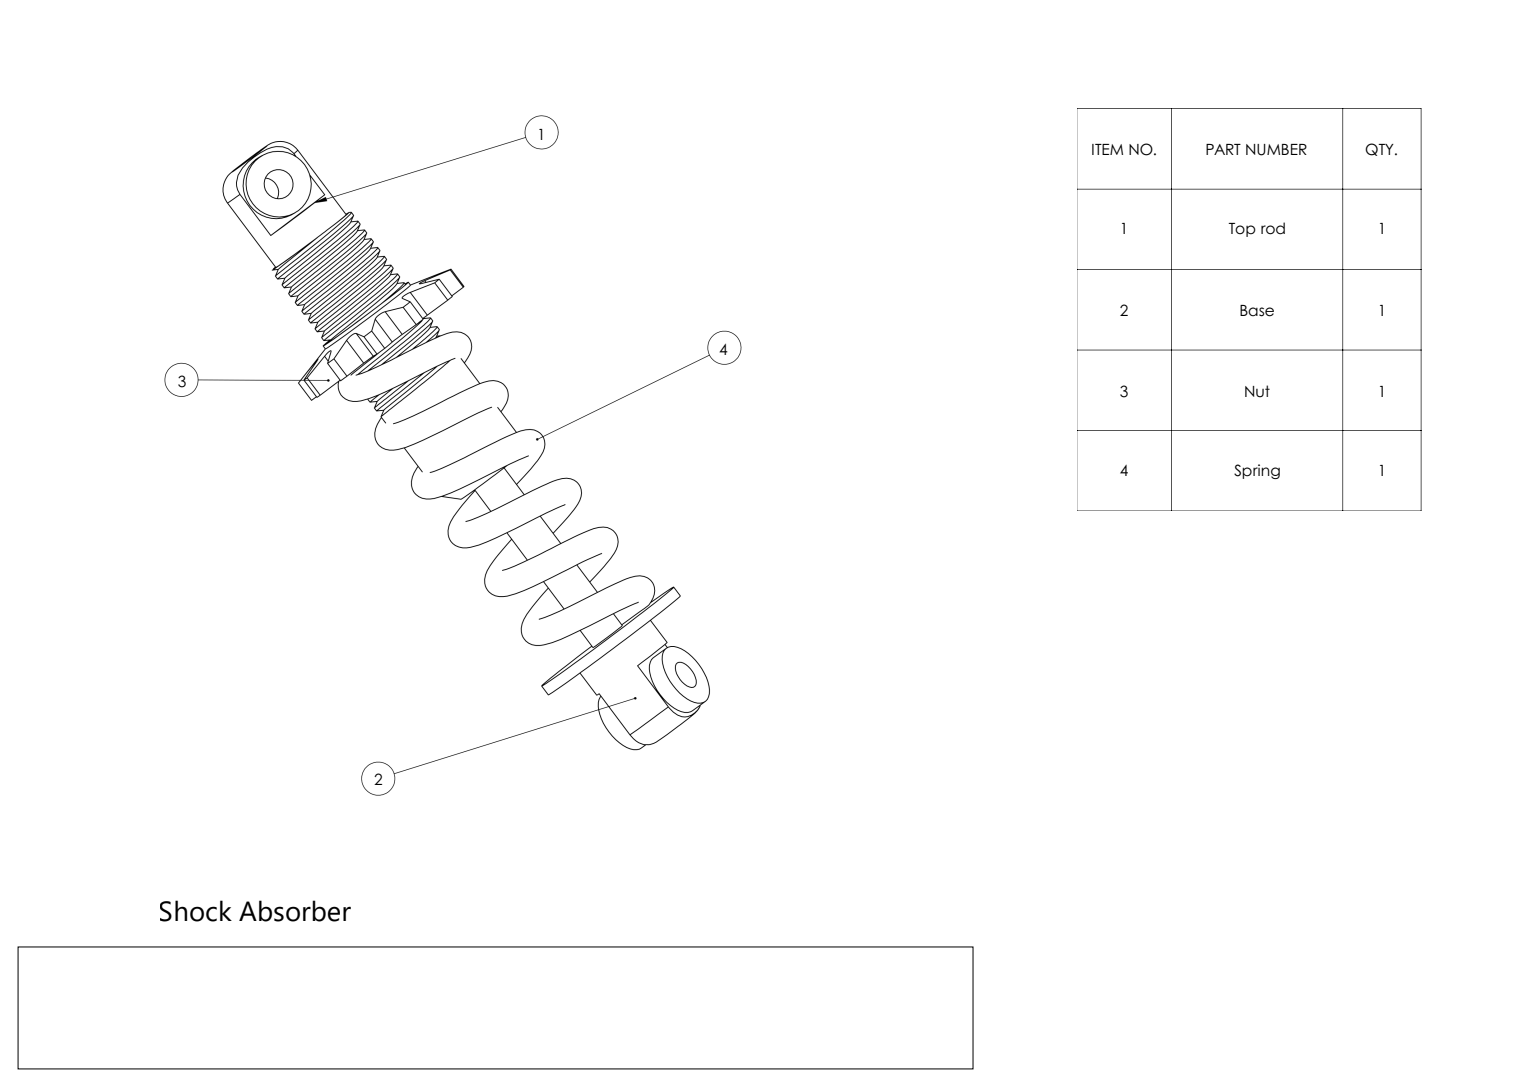
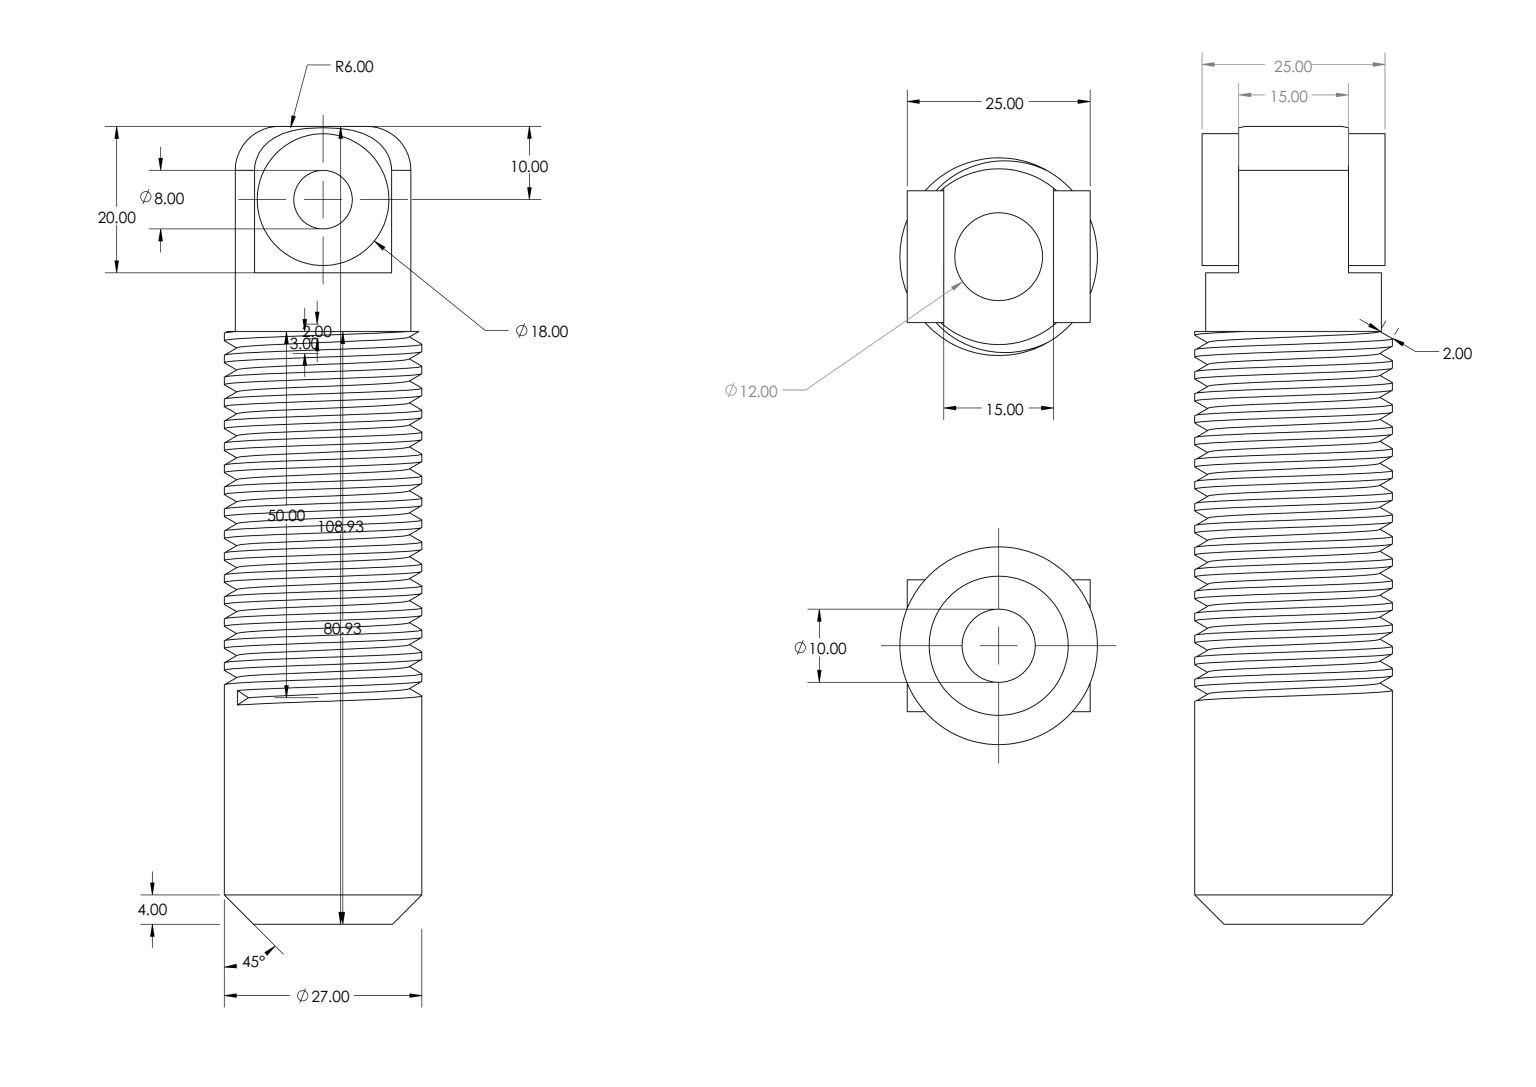
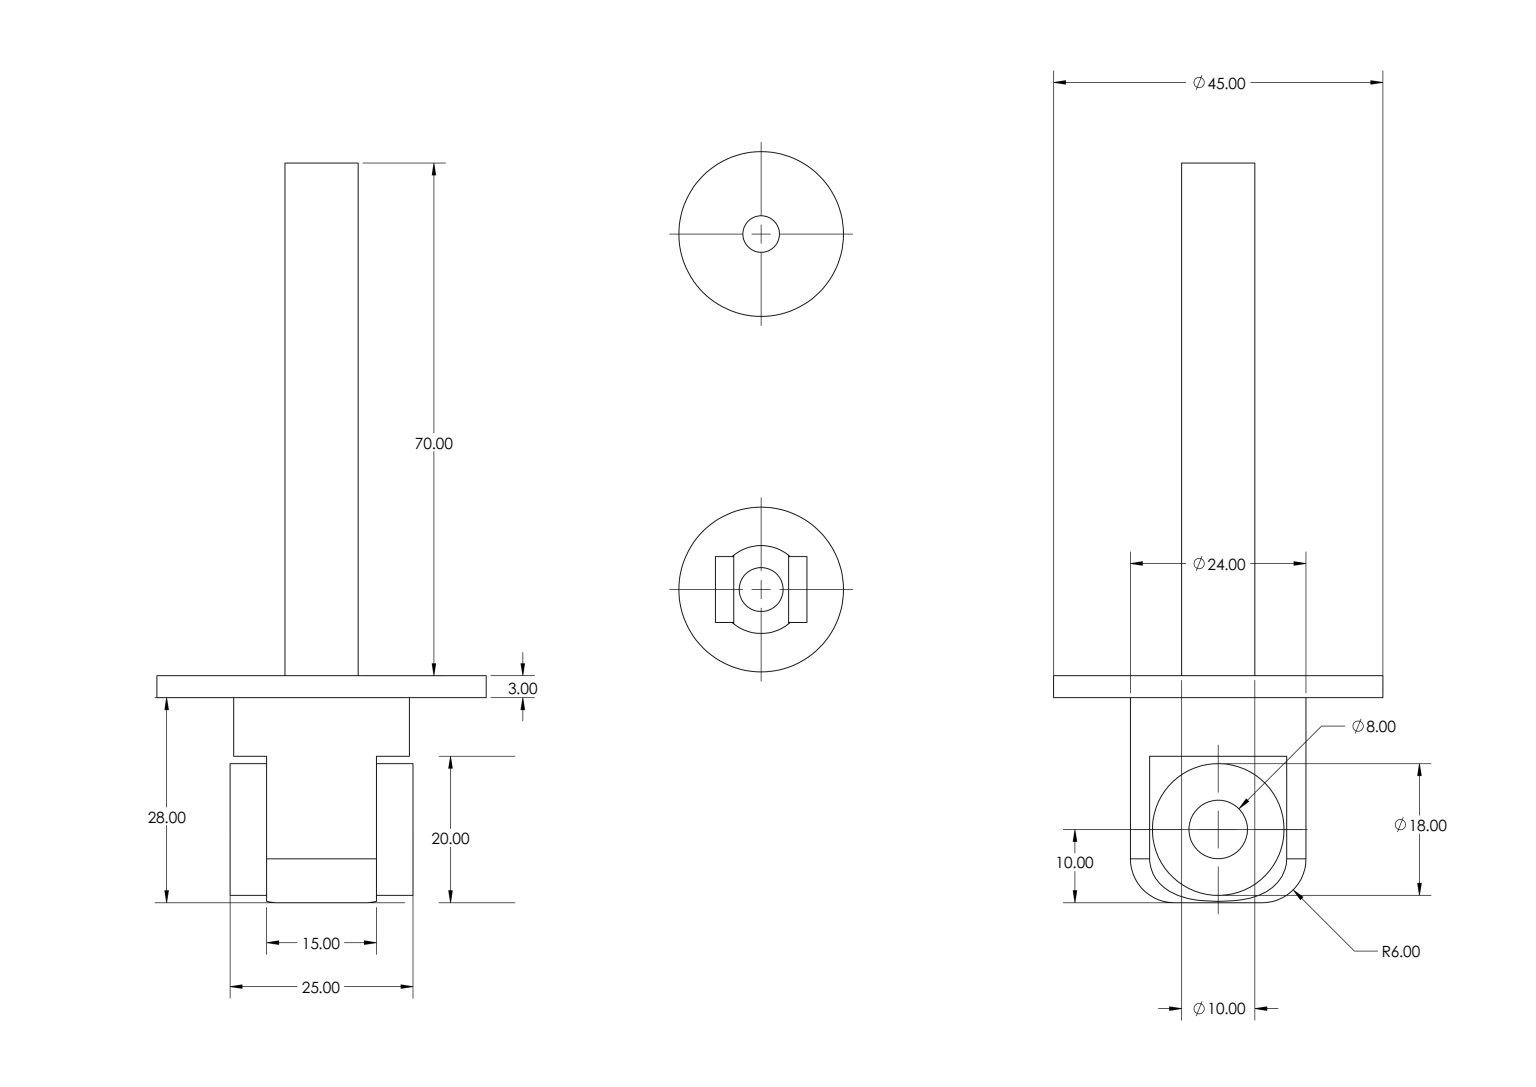
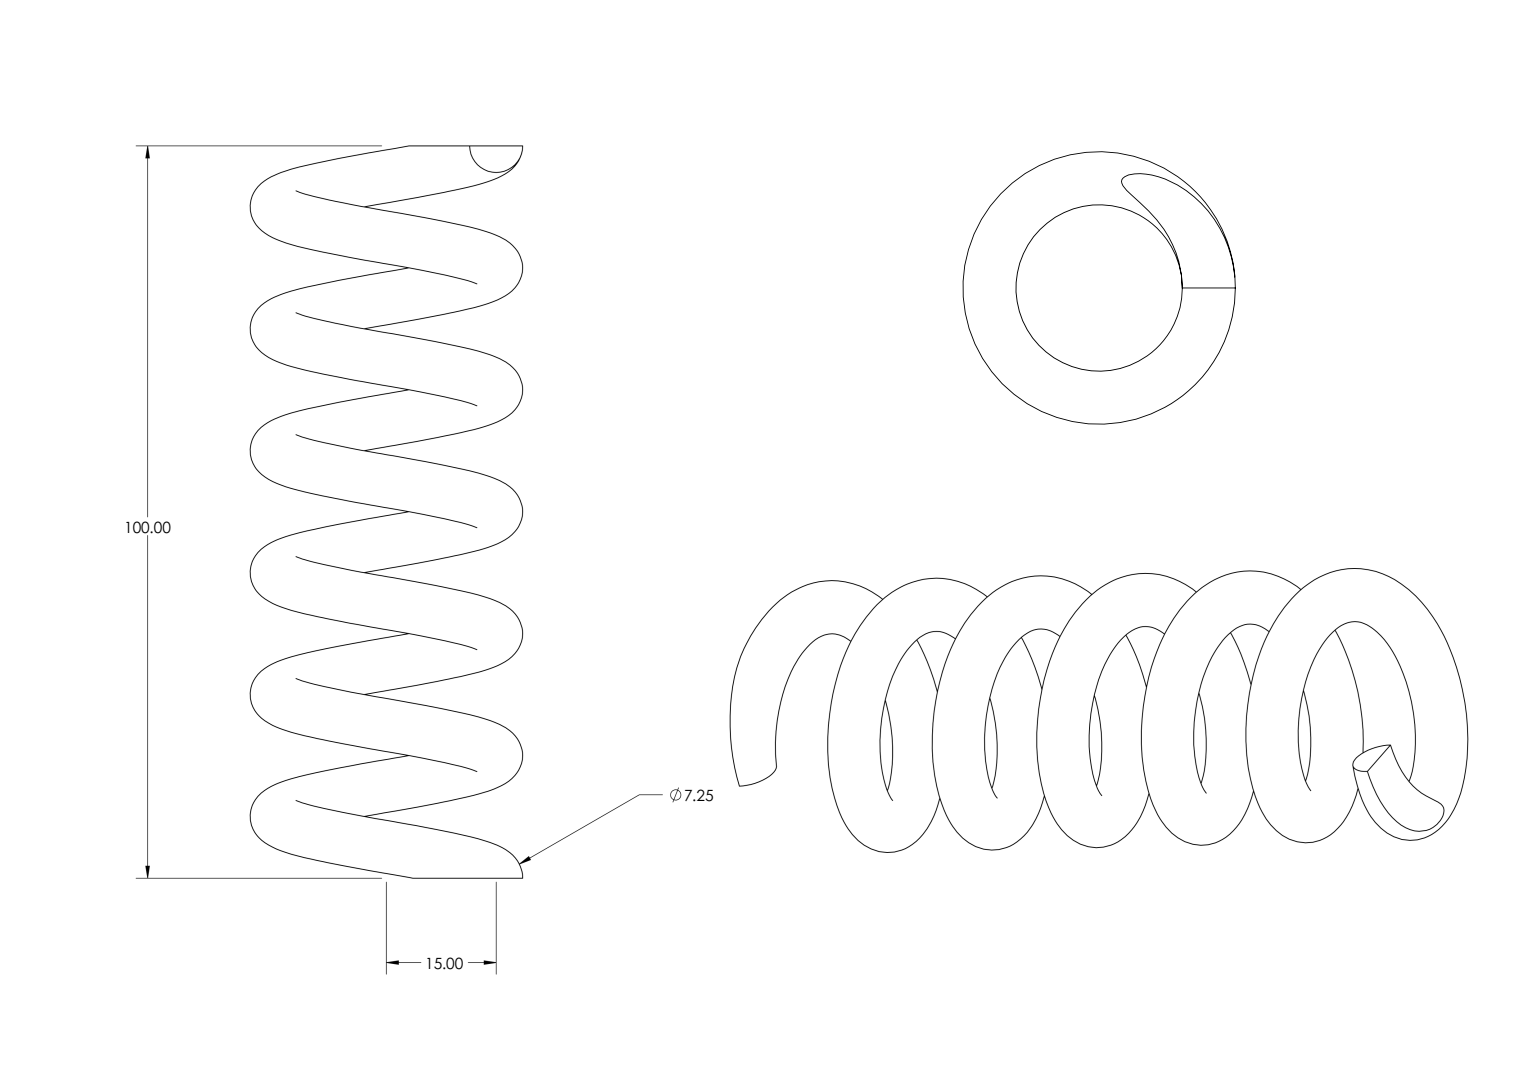
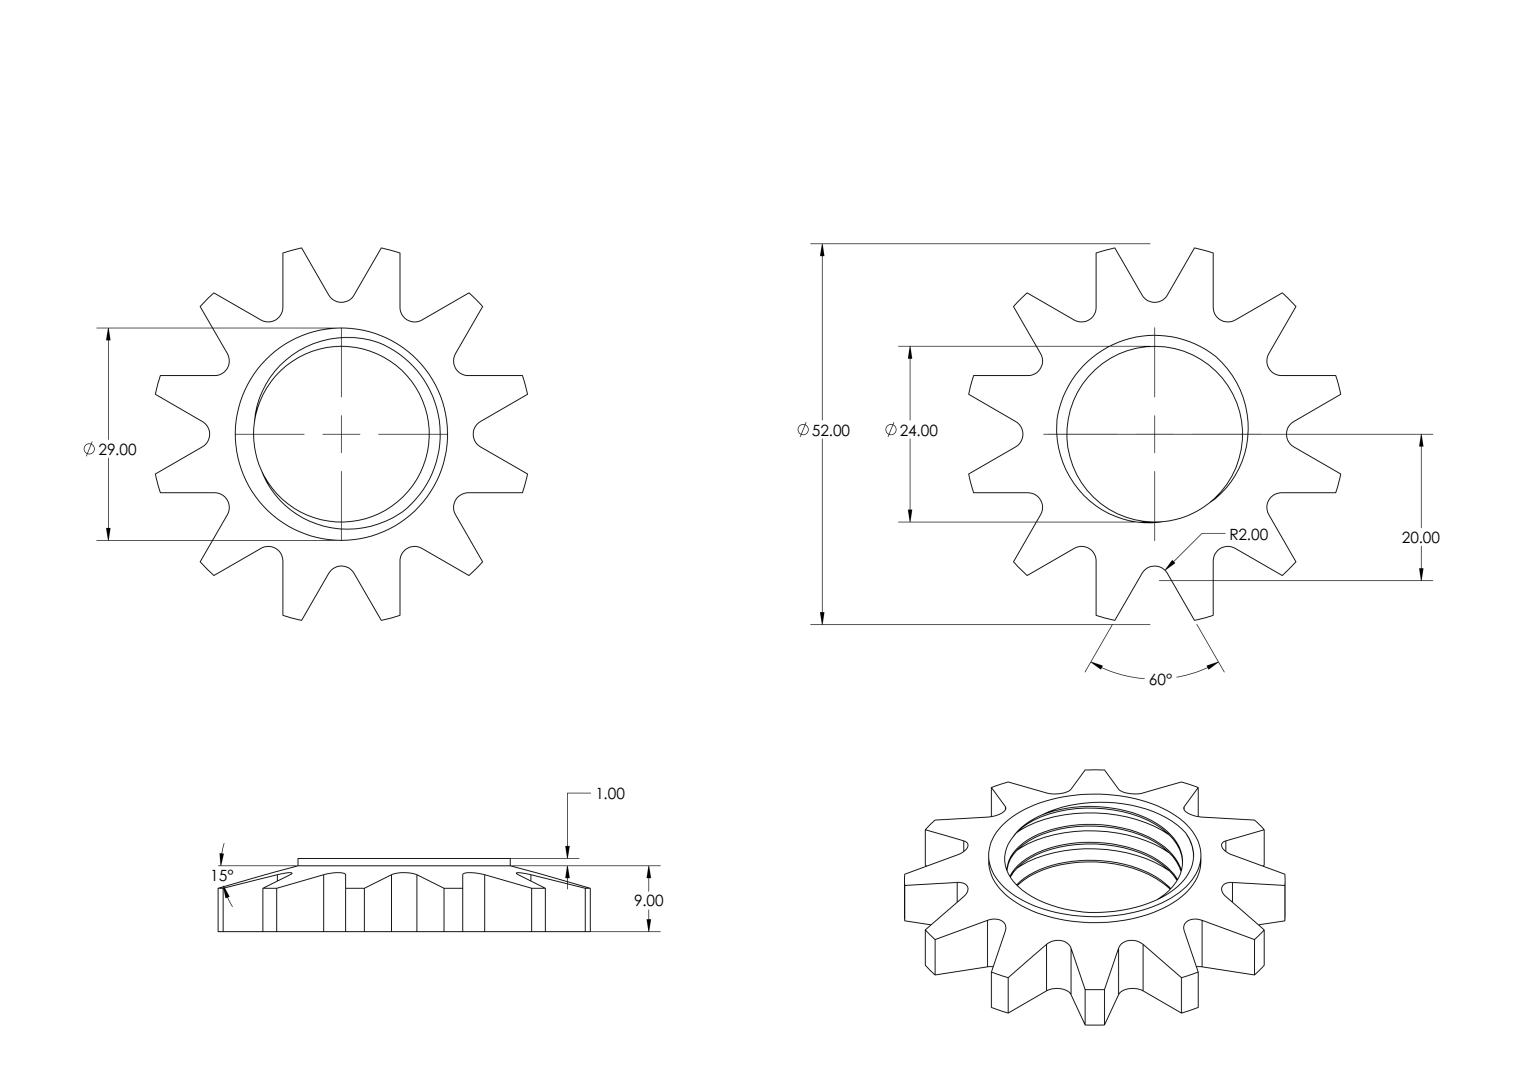
ISO-10303-21;
HEADER;
FILE_DESCRIPTION (('STEP AP214'),
    '1' );
FILE_NAME ('MAT-049',
    '2026-10-21T18:31:44',
    ( '' ),
    ( '' ),
    'SwSTEP 2.0',
    'SolidWorks 2025',
    '' );
FILE_SCHEMA (( 'AUTOMOTIVE_DESIGN' ));
ENDSEC;

DATA;
#1 = CARTESIAN_POINT ( 'NONE',  ( 6.241811971030540640, 75.95141910118948658, -11.97037661190906910 ) ) ;
#2 = CARTESIAN_POINT ( 'NONE',  ( 12.50000000000000000, 98.93000000000002103, 1.224646799147353059E-15 ) ) ;
#3 = CARTESIAN_POINT ( 'NONE',  ( 7.272992578804308828, 36.97999999999998977, 10.01041549318726709 ) ) ;
#4 = CARTESIAN_POINT ( 'NONE',  ( -4.562425571675021274, 41.51584201689734499, 12.70716777987128054 ) ) ;
#5 = CARTESIAN_POINT ( 'NONE',  ( -12.91556685892874867, 58.78902204722160718, -3.932462553950937689 ) ) ;
#6 = CARTESIAN_POINT ( 'NONE',  ( 4.630764260054621495, 44.84669919125740734, 12.68093428297014569 ) ) ;
#7 = CARTESIAN_POINT ( 'NONE',  ( -10.92172942406178926, 54.62999999999999545, -7.935100905948389460 ) ) ;
#8 = CARTESIAN_POINT ( 'NONE',  ( 8.860164440870203606, 30.02243855473401979, 10.18733757369393267 ) ) ;
#9 = ADVANCED_FACE ( 'NONE', ( #480 ), #9607, .F. ) ;
#10 = CARTESIAN_POINT ( 'NONE',  ( -27.07453251570901642, -8.000000000000003553, -22.50000000000000355 ) ) ;
#11 = CARTESIAN_POINT ( 'NONE',  ( -7.522916883230899465, 49.46192173470914355, -11.20972055436655523 ) ) ;
#12 = CARTESIAN_POINT ( 'NONE',  ( 10.11047073980464361, 63.77503176193906143, -8.949362642739272289 ) ) ;
#13 = CARTESIAN_POINT ( 'NONE',  ( 10.29443543732497979, 42.76512297172600796, -8.733575356815638457 ) ) ;
#14 = CARTESIAN_POINT ( 'NONE',  ( 1.387885517463281371, 38.72990328888538869, 13.42850322618521552 ) ) ;
#15 = EDGE_LOOP ( 'NONE', ( #14246, #2278, #8260, #10211 ) ) ;
#16 = DIRECTION ( 'NONE',  ( 0.000000000000000000, 0.000000000000000000, -1.000000000000000000 ) ) ;
#17 = CARTESIAN_POINT ( 'NONE',  ( -10.92172942406179104, 49.23000000000000398, 7.935100905948387684 ) ) ;
#18 = EDGE_LOOP ( 'NONE', ( #8634, #13740, #2829, #14978 ) ) ;
#19 = VERTEX_POINT ( 'NONE', #8191 ) ;
#20 = CARTESIAN_POINT ( 'NONE',  ( -8.549982208541774191E-16, 26.68000000000000682, 14.19474002721660355 ) ) ;
#21 = CARTESIAN_POINT ( 'NONE',  ( -13.16986379959834252, -72.84374999999981526, -13.16986379960055054 ) ) ;
#22 = CARTESIAN_POINT ( 'NONE',  ( 4.958471358563230069, 61.00121407256968098, -12.55670518402642521 ) ) ;
#23 = CARTESIAN_POINT ( 'NONE',  ( -4.171729424061787483, 8.330000000000003624, -12.83926296998457417 ) ) ;
#24 = CARTESIAN_POINT ( 'NONE',  ( 10.50943839410675196, 72.10666813338646364, 8.474155960609857985 ) ) ;
#25 = CARTESIAN_POINT ( 'NONE',  ( 12.25135822064244628, 57.63786423219936239, -5.672709418904434031 ) ) ;
#26 = CARTESIAN_POINT ( 'NONE',  ( 11.76794919243112325, 70.43000000000000682, 1.441158131103945434E-15 ) ) ;
#27 = CARTESIAN_POINT ( 'NONE',  ( 9.520470885617715595, 76.13000000000000966, 6.917026985038134512 ) ) ;
#28 = CARTESIAN_POINT ( 'NONE',  ( -7.237012465003837214, 47.41034925122353627, 11.39682853042513422 ) ) ;
#29 = CARTESIAN_POINT ( 'NONE',  ( -10.92172942406178926, 45.62999999999999545, -7.935100905948389460 ) ) ;
#30 = CARTESIAN_POINT ( 'NONE',  ( 7.347880794884122694E-16, 0.000000000000000000, -20.00000000000000000 ) ) ;
#31 = CARTESIAN_POINT ( 'NONE',  ( 10.92172942406178926, 38.12999999999999545, 7.935100905948387684 ) ) ;
#32 = CARTESIAN_POINT ( 'NONE',  ( 15.00000000000000000, -99.89999999999999147, 0.000000000000000000 ) ) ;
#33 = CARTESIAN_POINT ( 'NONE',  ( -11.37500000000000178, -84.32499999999977547, -9.545674412382054647E-13 ) ) ;
#34 =( BOUNDED_CURVE ( )  B_SPLINE_CURVE ( 2, ( #9058, #4723, #3556 ),
 .UNSPECIFIED., .F., .F. ) 
 B_SPLINE_CURVE_WITH_KNOTS ( ( 3, 3 ),
 ( 0.6250000000000000000, 0.6258333417219855699 ),
 .UNSPECIFIED. ) 
 CURVE ( )  GEOMETRIC_REPRESENTATION_ITEM ( )  RATIONAL_B_SPLINE_CURVE ( ( 0.9755282581475768211, 0.9755282581475767101, 0.9777307592560633420 ) ) 
 REPRESENTATION_ITEM ( '' )  );
#35 = CARTESIAN_POINT ( 'NONE',  ( 13.49999999999999822, 6.279999999999996696, 4.386415899144236796 ) ) ;
#36 = CARTESIAN_POINT ( 'NONE',  ( 11.39480283653290194, 33.70102987876868639, -7.239802240102667596 ) ) ;
#37 = CARTESIAN_POINT ( 'NONE',  ( -4.107118796296879815, 73.32755911965604412, -12.86190453662493383 ) ) ;
#38 = ORIENTED_EDGE ( 'NONE', *, *, #7659, .T. ) ;
#39 = VERTEX_POINT ( 'NONE', #5535 ) ;
#40 = CARTESIAN_POINT ( 'NONE',  ( 11.76794919243112680, 26.57999999999999829, -3.823638476888993942 ) ) ;
#41 = CARTESIAN_POINT ( 'NONE',  ( -2.167727191357447403, 62.60205656133668839, 13.32483508987561649 ) ) ;
#42 = VERTEX_POINT ( 'NONE', #221 ) ;
#43 = CARTESIAN_POINT ( 'NONE',  ( -13.33648623469416528, 41.00345850548239213, 2.095001394486209367 ) ) ;
#44 = CARTESIAN_POINT ( 'NONE',  ( 9.520470885617717371, -12.26999999999999602, -6.917026985038131848 ) ) ;
#45 = CARTESIAN_POINT ( 'NONE',  ( 8.043339635996298753, -88.41874999999980389, 8.043339635997652337 ) ) ;
#46 = CARTESIAN_POINT ( 'NONE',  ( -12.68486621467936359, 44.09791772264757270, 4.641127458682580809 ) ) ;
#47 = CARTESIAN_POINT ( 'NONE',  ( 12.50000000000000000, 98.93000000000002103, 1.224646799147353059E-15 ) ) ;
#48 = PRODUCT_DEFINITION ( 'UNKNOWN', '', #15519, #4010 ) ;
#49 = CARTESIAN_POINT ( 'NONE',  ( -4.171729424061787483, 46.32999999999999829, -12.83926296998457417 ) ) ;
#50 = CARTESIAN_POINT ( 'NONE',  ( 10.92172942406178926, 44.13000000000000256, 7.935100905948387684 ) ) ;
#51 = CARTESIAN_POINT ( 'NONE',  ( -12.09611347903164891, 71.15127006308296131, 6.013594338244640625 ) ) ;
#52 = CARTESIAN_POINT ( 'NONE',  ( 7.714727599200456254, -45.82187499999987779, -18.62499999999935341 ) ) ;
#53 = EDGE_CURVE ( 'NONE', #3761, #17169, #15927, .T. ) ;
#54 = CARTESIAN_POINT ( 'NONE',  ( -13.10508471444031287, 68.04691603053561266, 3.289941233735407256 ) ) ;
#55 = CARTESIAN_POINT ( 'NONE',  ( -7.714727599197334307, 2.046875000000014211, -18.62500000000064659 ) ) ;
#56 = EDGE_CURVE ( 'NONE', #7801, #2957, #9184, .T. ) ;
#57 = CARTESIAN_POINT ( 'NONE',  ( 13.49788837497377969, 54.40198127425698971, 0.8139535183936712492 ) ) ;
#58 = DIRECTION ( 'NONE',  ( -0.000000000000000000, -1.000000000000000000, -0.000000000000000000 ) ) ;
#59 = CARTESIAN_POINT ( 'NONE',  ( -11.88785451664102411, 64.69331280751505631, -6.397572128427487570 ) ) ;
#60 = DIRECTION ( 'NONE',  ( 0.4999999999999977240, 0.000000000000000000, 0.8660254037844399289 ) ) ;
#61 = CARTESIAN_POINT ( 'NONE',  ( -13.32240026865723692, 35.00664116012176663, 2.183159191248645659 ) ) ;
#62 = CARTESIAN_POINT ( 'NONE',  ( 10.92172942406179104, 19.72999999999999687, -7.935100905948385908 ) ) ;
#63 = ORIENTED_EDGE ( 'NONE', *, *, #6522, .T. ) ;
#64 = CARTESIAN_POINT ( 'NONE',  ( -12.94117117538681683, 4.250271015223984582E-15, -2.797136868549697564 ) ) ;
#65 = CARTESIAN_POINT ( 'NONE',  ( -1.332730275901221395, 31.22788502858077209, -13.43591754810035432 ) ) ;
#66 = CARTESIAN_POINT ( 'NONE',  ( 2.964303633682398686, 73.07342191280697818, -13.17196784541496513 ) ) ;
#67 = CARTESIAN_POINT ( 'NONE',  ( -11.76794919243112325, -7.919999999999998153, 3.823638476888994386 ) ) ;
#68 = DIRECTION ( 'NONE',  ( 0.000000000000000000, 0.000000000000000000, 1.000000000000000000 ) ) ;
#69 = CARTESIAN_POINT ( 'NONE',  ( -4.171729424061791036, -11.47000000000000064, 12.83926296998457239 ) ) ;
#70 = CARTESIAN_POINT ( 'NONE',  ( -12.68834643456797906, 52.76331015659336998, -4.610928276790117408 ) ) ;
#71 = CIRCLE ( 'NONE', #15856, 9.000000000000000000 ) ;
#72 = CARTESIAN_POINT ( 'NONE',  ( 9.520470885617715595, 46.12999999999999545, 6.917026985038134512 ) ) ;
#73 = CARTESIAN_POINT ( 'NONE',  ( 3.294673121883986422, 50.79846311650262436, 13.09179671531762246 ) ) ;
#74 = CARTESIAN_POINT ( 'NONE',  ( -9.961542587724716569, 37.57728390915936956, -9.113131270120877758 ) ) ;
#75 = EDGE_CURVE ( 'NONE', #10985, #13128, #6860, .T. ) ;
#76 = CARTESIAN_POINT ( 'NONE',  ( 10.08038093372313604, 36.08304225860660353, 8.991274832604577938 ) ) ;
#77 = CARTESIAN_POINT ( 'NONE',  ( 8.043339635996298753, -105.0687499999997527, 8.043339635997652337 ) ) ;
#78 = CARTESIAN_POINT ( 'NONE',  ( -11.44756249950965632, 74.19779003843927967, 7.160551751645796159 ) ) ;
#79 = CARTESIAN_POINT ( 'NONE',  ( -13.19858737197696286, 77.03056283200281484, 2.845309594670863973 ) ) ;
#80 = AXIS2_PLACEMENT_3D ( 'NONE', #263, #10869, #2892 ) ;
#81 = CARTESIAN_POINT ( 'NONE',  ( -6.071462803580223166, 79.40141861843632398, -12.06817019399647783 ) ) ;
#82 = CARTESIAN_POINT ( 'NONE',  ( 2.279995255611139653E-15, 9.179999999999992610, -12.37355403259654985 ) ) ;
#83 = CARTESIAN_POINT ( 'NONE',  ( 13.50000000000000000, 4.430000000000003268, 1.734723475976807094E-15 ) ) ;
#84 = CARTESIAN_POINT ( 'NONE',  ( 1.982521523170245906E-06, 77.68005525700222336, 13.49999999999970690 ) ) ;
#85 = CARTESIAN_POINT ( 'NONE',  ( 11.76794919243112680, -0.4200000000000027045, -3.823638476888993942 ) ) ;
#86 = CARTESIAN_POINT ( 'NONE',  ( 3.636496289402154414, 51.82999999999999829, 11.19198476289190936 ) ) ;
#87 = CARTESIAN_POINT ( 'NONE',  ( 8.043339635997654113, -18.73124999999995666, -8.043339635996304082 ) ) ;
#88 = CARTESIAN_POINT ( 'NONE',  ( -13.16986379960055231, -43.70624999999989768, 13.16986379959834252 ) ) ;
#89 = CARTESIAN_POINT ( 'NONE',  ( -10.92172942406179104, -12.76999999999999602, 7.935100905948385908 ) ) ;
#90 = CARTESIAN_POINT ( 'NONE',  ( -8.290587820170616240, 40.49598020429036183, -10.65487298274420525 ) ) ;
#91 = CARTESIAN_POINT ( 'NONE',  ( -2.747897566831316141, 34.27880424421546479, -13.21738048412783151 ) ) ;
#92 = CARTESIAN_POINT ( 'NONE',  ( 13.48604648626630542, 75.45114278836371113, -0.6137407349411325708 ) ) ;
#93 = CARTESIAN_POINT ( 'NONE',  ( 15.91271015948297141, 2.066541229842319115E-14, -9.178967570126440378 ) ) ;
#94 = CARTESIAN_POINT ( 'NONE',  ( -11.76794919243112325, 32.92999999999999972, -2.882316262207890869E-15 ) ) ;
#95 = CARTESIAN_POINT ( 'NONE',  ( -6.586690174280394494, 41.43750565762731952, 11.78692872275349579 ) ) ;
#96 = CARTESIAN_POINT ( 'NONE',  ( -4.171426067996565124, 58.32999100947719029, -12.83948131572000584 ) ) ;
#97 = CARTESIAN_POINT ( 'NONE',  ( 6.370293526262202022, 44.91380087981439573, 11.90272333445460262 ) ) ;
#98 = ADVANCED_FACE ( 'NONE', ( #16379 ), #12591, .T. ) ;
#99 = CARTESIAN_POINT ( 'NONE',  ( -17.32050807568884210, 7.773118517290098950, 7.999999999999840128 ) ) ;
#100 = CARTESIAN_POINT ( 'NONE',  ( 1.108954987895778950E-11, 4.813974596216015200, 12.00000000000000178 ) ) ;
#101 = CARTESIAN_POINT ( 'NONE',  ( -4.171729424061791036, 58.53000000000000114, 12.83926296998457239 ) ) ;
#102 = CARTESIAN_POINT ( 'NONE',  ( -11.20551244324089524, 49.64703832191597854, -7.529055542132852885 ) ) ;
#103 = CARTESIAN_POINT ( 'NONE',  ( 13.46801799936566724, 63.39787863554747815, 0.9304553811726751222 ) ) ;
#104 = CARTESIAN_POINT ( 'NONE',  ( 11.68815242529539411, 42.17840658691920908, 6.773979411268512330 ) ) ;
#105 = CARTESIAN_POINT ( 'NONE',  ( 4.417203864861311224, 38.83887425577129449, 12.75710294833973357 ) ) ;
#106 = VERTEX_POINT ( 'NONE', #2759 ) ;
#107 = CARTESIAN_POINT ( 'NONE',  ( -4.026122579657434919, 70.32476532614168718, -12.88571505164192033 ) ) ;
#108 = CARTESIAN_POINT ( 'NONE',  ( -13.49999999999999822, 48.77999999999998693, -4.386415899144240349 ) ) ;
#109 = CARTESIAN_POINT ( 'NONE',  ( -8.343458848123582072, 14.37999999999998835, 11.48378591275254124 ) ) ;
#110 = EDGE_LOOP ( 'NONE', ( #6207, #1537, #1550, #818 ) ) ;
#111 = CARTESIAN_POINT ( 'NONE',  ( -4.477815178396856055, 43.34114203380904229, -12.73627368523690606 ) ) ;
#112 = DIRECTION ( 'NONE',  ( -0.000000000000000000, -1.000000000000000000, -0.000000000000000000 ) ) ;
#113 = CARTESIAN_POINT ( 'NONE',  ( 6.392086272904786703, 60.94536626219394293, -11.89080869004308205 ) ) ;
#114 = CARTESIAN_POINT ( 'NONE',  ( -8.343458848123576743, 14.47999999999999865, -11.48378591275254301 ) ) ;
#115 = CARTESIAN_POINT ( 'NONE',  ( 2.453092984686562339, 71.76820780413271450, 13.27525308931726578 ) ) ;
#116 = CARTESIAN_POINT ( 'NONE',  ( 13.40373713238982489, 66.48610201136790465, -1.609300758946977661 ) ) ;
#117 = CARTESIAN_POINT ( 'NONE',  ( 4.966293671374200969, 56.85915651247563574, 12.55332637815666708 ) ) ;
#118 = CARTESIAN_POINT ( 'NONE',  ( 3.636496289402154414, 66.82999999999999829, 11.19198476289190936 ) ) ;
#119 = CARTESIAN_POINT ( 'NONE',  ( 9.520470885617715595, 64.12999999999999545, 6.917026985038134512 ) ) ;
#120 = CARTESIAN_POINT ( 'NONE',  ( -3.966664967154714727, 47.53736456333449922, 12.90422583550607527 ) ) ;
#121 = CARTESIAN_POINT ( 'NONE',  ( -13.49999999999999822, 45.78000000000000114, -4.386415899144240349 ) ) ;
#122 = CARTESIAN_POINT ( 'NONE',  ( -8.224360503536546367E-15, 78.17999999999999261, -13.50000000000000000 ) ) ;
#123 = CARTESIAN_POINT ( 'NONE',  ( 4.163872747629839388, -100.0000000000000426, 15.14667126703698585 ) ) ;
#124 = CARTESIAN_POINT ( 'NONE',  ( -3.802315511192875697, 56.54328190446157976, 12.95363457325665202 ) ) ;
#125 = CARTESIAN_POINT ( 'NONE',  ( -11.37500000000000000, -41.62499999999990052, -9.545674412382054647E-13 ) ) ;
#126 = CARTESIAN_POINT ( 'NONE',  ( -4.171729424061791036, 40.52999999999999403, 12.83926296998457239 ) ) ;
#127 = AXIS2_PLACEMENT_3D ( 'NONE', #2848, #1623, #9520 ) ;
#128 = CARTESIAN_POINT ( 'NONE',  ( 13.48850798719686317, 33.44917238739969889, -0.5569197484580091784 ) ) ;
#129 = CARTESIAN_POINT ( 'NONE',  ( -13.14483242576192978, 7.170662809914418290, -16.82677684650047567 ) ) ;
#130 = EDGE_LOOP ( 'NONE', ( #12331, #307, #5558 ) ) ;
#131 = EDGE_LOOP ( 'NONE', ( #5447, #10898, #7879, #3829 ) ) ;
#132 = CARTESIAN_POINT ( 'NONE',  ( -2.372100534622330059, 62.59470822479858043, 13.29057958102706571 ) ) ;
#133 = ORIENTED_EDGE ( 'NONE', *, *, #911, .F. ) ;
#134 = B_SPLINE_CURVE_WITH_KNOTS ( 'NONE', 3,
 ( #15432, #7424, #3341, #16438 ),
 .UNSPECIFIED., .F., .F.,
 ( 4, 4 ),
 ( 2.376698214938428888E-07, 0.007646667280170321192 ),
 .UNSPECIFIED. ) ;
#135 = CARTESIAN_POINT ( 'NONE',  ( -11.76794919243112325, -14.22000000000000242, -3.823638476888998827 ) ) ;
#136 = CARTESIAN_POINT ( 'NONE',  ( 13.16986379960055409, -42.63124999999990905, -13.16986379959834430 ) ) ;
#137 = CARTESIAN_POINT ( 'NONE',  ( -13.22798356179965751, 44.02531610866294187, 2.697370474855687927 ) ) ;
#138 = CARTESIAN_POINT ( 'NONE',  ( 7.999999999999904965, 7.773118517290098950, 17.32050807568881368 ) ) ;
#139 = EDGE_CURVE ( 'NONE', #3044, #15045, #14019, .T. ) ;
#140 = CARTESIAN_POINT ( 'NONE',  ( 13.50000000000000355, 42.57999999999999829, -4.386415899144233244 ) ) ;
#141 = CARTESIAN_POINT ( 'NONE',  ( -13.50000000000000000, 48.92999999999999972, -3.306546357697853733E-15 ) ) ;
#142 = CARTESIAN_POINT ( 'NONE',  ( -13.48995242675199790, 70.94917795696534313, 0.5552773507619721549 ) ) ;
#143 =( BOUNDED_CURVE ( )  B_SPLINE_CURVE ( 1, ( #8817, #14343 ),
 .UNSPECIFIED., .F., .F. ) 
 B_SPLINE_CURVE_WITH_KNOTS ( ( 2, 2 ),
 ( 0.000000000000000000, 1.000000000000000000 ),
 .UNSPECIFIED. ) 
 CURVE ( )  GEOMETRIC_REPRESENTATION_ITEM ( )  RATIONAL_B_SPLINE_CURVE ( ( 0.9782075210486875783, 0.9782075210486875783 ) ) 
 REPRESENTATION_ITEM ( '' )  );
#144 = CARTESIAN_POINT ( 'NONE',  ( -13.16986379959834252, -65.59374999999981526, -13.16986379960055409 ) ) ;
#145 = CARTESIAN_POINT ( 'NONE',  ( -11.47846244632648549, 67.66437547590606982, -7.110784611987690518 ) ) ;
#146 = CARTESIAN_POINT ( 'NONE',  ( 18.62500000000000000, -75.99999999999980105, 1.560692158462880521E-12 ) ) ;
#147 = CARTESIAN_POINT ( 'NONE',  ( 12.45812093344438587, 54.62011758101717618, -5.223734028880926417 ) ) ;
#148 = CARTESIAN_POINT ( 'NONE',  ( -11.89319909969382039, 64.69371209007049117, -6.387634285403382073 ) ) ;
#149 = VERTEX_POINT ( 'NONE', #9845 ) ;
#150 = CARTESIAN_POINT ( 'NONE',  ( 15.58845726811991916, 7.773118517290098950, -10.99999999999996092 ) ) ;
#151 = CARTESIAN_POINT ( 'NONE',  ( -12.98939268596651786, 34.79855291303425702, -3.677969189785255555 ) ) ;
#152 = ORIENTED_EDGE ( 'NONE', *, *, #6438, .T. ) ;
#153 = CARTESIAN_POINT ( 'NONE',  ( 13.08478391751391001, 78.54823588313601590, -3.322629509287643224 ) ) ;
#154 = CARTESIAN_POINT ( 'NONE',  ( -13.39378209699495592, -2.969872329747732787E-15, 1.511216576358205943 ) ) ;
#155 = CARTESIAN_POINT ( 'NONE',  ( 0.000000000000000000, 73.00000000000001421, 0.000000000000000000 ) ) ;
#156 = CARTESIAN_POINT ( 'NONE',  ( -9.949531856098463578, 31.57665661914821342, -9.126009350303103673 ) ) ;
#157 = CARTESIAN_POINT ( 'NONE',  ( 10.34601424054412000, 72.76232993950749517, -8.672412499177319489 ) ) ;
#158 = CARTESIAN_POINT ( 'NONE',  ( -7.409984580736203970E-16, -7.320000000000002949, 12.37355403259654985 ) ) ;
#159 = DIRECTION ( 'NONE',  ( 1.000000000000000000, 0.000000000000000000, 0.000000000000000000 ) ) ;
#160 = EDGE_CURVE ( 'NONE', #16949, #8284, #16780, .T. ) ;
#161 = CARTESIAN_POINT ( 'NONE',  ( -4.171729424061791036, -14.46999999999999709, 12.83926296998457239 ) ) ;
#162 = AXIS2_PLACEMENT_3D ( 'NONE', #175, #4418, #13594 ) ;
#163 = CARTESIAN_POINT ( 'NONE',  ( -10.92172942406178926, 70.62999999999999545, -7.935100905948389460 ) ) ;
#164 = CARTESIAN_POINT ( 'NONE',  ( -12.03726189314226858, 53.15526546510770345, 6.112069937274645426 ) ) ;
#165 = CARTESIAN_POINT ( 'NONE',  ( -7.272992578804307939, 44.47999999999999687, -10.01041549318726886 ) ) ;
#166 = CARTESIAN_POINT ( 'NONE',  ( -13.50000000000000000, 69.93000000000000682, -3.306546357697853733E-15 ) ) ;
#167 = CARTESIAN_POINT ( 'NONE',  ( -16.03540712409196090, 8.027799080943070820, -8.457499700851245805 ) ) ;
#168 = CARTESIAN_POINT ( 'NONE',  ( 11.95757905990039127, 69.66142261759961229, -6.266300119430860072 ) ) ;
#169 = CARTESIAN_POINT ( 'NONE',  ( -4.427829777958112167, 37.33925957768354920, -12.75364605705754606 ) ) ;
#170 = CARTESIAN_POINT ( 'NONE',  ( 3.589871069019304972, 35.80905818983445954, 13.01962489795650768 ) ) ;
#171 = CARTESIAN_POINT ( 'NONE',  ( -11.37500000000039613, -83.21562499999981810, 4.711679271993000739 ) ) ;
#172 = CARTESIAN_POINT ( 'NONE',  ( -10.34620055824173868, 74.26233662262045243, 8.672923399463462246 ) ) ;
#173 = CARTESIAN_POINT ( 'NONE',  ( -13.29880297559754609, 76.84835896960053958, -2.322037454927736277 ) ) ;
#174 = DIRECTION ( 'NONE',  ( 0.000000000000000000, -1.000000000000000000, 0.000000000000000000 ) ) ;
#175 = CARTESIAN_POINT ( 'NONE',  ( 0.000000000000000000, 0.000000000000000000, 0.000000000000000000 ) ) ;
#176 = CARTESIAN_POINT ( 'NONE',  ( -8.380961239563070819, 80.93000000000004945, 9.227099233226635278 ) ) ;
#177 = CARTESIAN_POINT ( 'NONE',  ( 13.49999999999999822, 28.28000000000000114, 4.386415899144237684 ) ) ;
#178 = CARTESIAN_POINT ( 'NONE',  ( -11.76794919243112325, 4.080000000000008065, 3.823638476888994386 ) ) ;
#179 = CARTESIAN_POINT ( 'NONE',  ( 9.520470885617715595, 46.12999999999999545, 6.917026985038134512 ) ) ;
#180 = CARTESIAN_POINT ( 'NONE',  ( 13.49999999999999822, -17.72000000000000242, 4.386415899144237684 ) ) ;
#181 = CARTESIAN_POINT ( 'NONE',  ( 6.750022565184456980, 31.92926174983938026, 11.69132992304556495 ) ) ;
#182 = CARTESIAN_POINT ( 'NONE',  ( 10.14927042510883481, 75.08716984626934732, 8.902032665787164234 ) ) ;
#183 = EDGE_CURVE ( 'NONE', #10985, #14307, #6879, .T. ) ;
#184 = CARTESIAN_POINT ( 'NONE',  ( 3.512344863372272030, -7.135244913870580524E-13, -15.22848700163195623 ) ) ;
#185 = VECTOR ( 'NONE', #11440, 1000.000000000000000 ) ;
#186 = CARTESIAN_POINT ( 'NONE',  ( 0.000000000000000000, 0.000000000000000000, 0.000000000000000000 ) ) ;
#187 = CARTESIAN_POINT ( 'NONE',  ( -6.864354898698485918, 41.42600474588421378, 11.62474807620217376 ) ) ;
#188 = CARTESIAN_POINT ( 'NONE',  ( -6.117255243659908359, 58.40366678541308687, -12.03616728541428493 ) ) ;
#189 = FACE_OUTER_BOUND ( 'NONE', #3646, .T. ) ;
#190 = CARTESIAN_POINT ( 'NONE',  ( -4.171729424061787483, 54.33000000000000540, -12.83926296998457417 ) ) ;
#191 = DIRECTION ( 'NONE',  ( -0.000000000000000000, -1.000000000000000000, -0.000000000000000000 ) ) ;
#192 = CARTESIAN_POINT ( 'NONE',  ( -13.49999999999999822, 57.78000000000000114, -4.386415899144240349 ) ) ;
#193 = CARTESIAN_POINT ( 'NONE',  ( -11.00427691244374273, 49.63475489259692353, -7.821558401853768494 ) ) ;
#194 = CARTESIAN_POINT ( 'NONE',  ( 11.36089011803204407, 63.70299262790948802, -7.293906877826991320 ) ) ;
#195 = CARTESIAN_POINT ( 'NONE',  ( 13.46351984225201548, 42.39558882709123111, 0.9962785372066437217 ) ) ;
#196 = CARTESIAN_POINT ( 'NONE',  ( 3.151611543758418676, 38.79326144612200267, 13.13455959399786899 ) ) ;
#197 = ORIENTED_EDGE ( 'NONE', *, *, #1177, .T. ) ;
#198 = CARTESIAN_POINT ( 'NONE',  ( -3.974014160384248928, 70.32289088885870854, -12.90183134154761113 ) ) ;
#199 = CARTESIAN_POINT ( 'NONE',  ( -11.37500000000039613, -9.365624999999976552, 4.711679271993001628 ) ) ;
#200 = CIRCLE ( 'NONE', #2424, 5.000000000000000000 ) ;
#201 = VERTEX_POINT ( 'NONE', #13114 ) ;
#202 = CARTESIAN_POINT ( 'NONE',  ( -11.06052376482290889, 43.63819014080397807, -7.740673448246946364 ) ) ;
#203 = CARTESIAN_POINT ( 'NONE',  ( -7.499999999999999112, 105.5999945338998174, 8.557281619885976909 ) ) ;
#204 = CARTESIAN_POINT ( 'NONE',  ( 10.49915709197846603, 60.75394407136035113, -8.486442428007933358 ) ) ;
#205 = CARTESIAN_POINT ( 'NONE',  ( 13.50000000000000355, 7.579999999999999183, -4.386415899144233244 ) ) ;
#206 = EDGE_CURVE ( 'NONE', #10449, #12592, #1531, .T. ) ;
#207 = CARTESIAN_POINT ( 'NONE',  ( -3.708203932499367195, 6.196025403784440222, -11.41267819554184548 ) ) ;
#208 = CARTESIAN_POINT ( 'NONE',  ( 12.91036043465679128, 66.57159231767617769, -3.948717839537223551 ) ) ;
#209 = CARTESIAN_POINT ( 'NONE',  ( 10.83372828063143523, 57.12494043467410165, 8.055071804621336540 ) ) ;
#210 = CARTESIAN_POINT ( 'NONE',  ( 3.636496289402157078, 62.03000000000000114, -11.19198476289190936 ) ) ;
#211 = CARTESIAN_POINT ( 'NONE',  ( -11.76794919243112325, 71.78000000000000114, -3.823638476888998827 ) ) ;
#212 = CARTESIAN_POINT ( 'NONE',  ( -8.395919747993797699, 47.35978594638820738, 10.59303779737377127 ) ) ;
#213 = CARTESIAN_POINT ( 'NONE',  ( -10.92172942406179104, 46.22999999999999687, 7.935100905948387684 ) ) ;
#214 = FACE_OUTER_BOUND ( 'NONE', #12871, .T. ) ;
#215 = CARTESIAN_POINT ( 'NONE',  ( 3.658660341103826763, -100.0000000000000000, 14.07150118901589408 ) ) ;
#216 = CARTESIAN_POINT ( 'NONE',  ( -9.167797302161076800, 56.32288307047150511, 9.914146655588314871 ) ) ;
#217 = CARTESIAN_POINT ( 'NONE',  ( 8.043339635996300530, -81.16874999999980389, 8.043339635997654113 ) ) ;
#218 = CARTESIAN_POINT ( 'NONE',  ( 2.138189944381238661, 5.756881422320270225, 13.49999999999999822 ) ) ;
#219 = CARTESIAN_POINT ( 'NONE',  ( 12.00723290083941208, 33.65759935958783444, -6.170612997742742856 ) ) ;
#220 = PLANE ( 'NONE',  #1477 ) ;
#221 = CARTESIAN_POINT ( 'NONE',  ( -18.99999999999998224, 0.000000000000000000, -1.732050807569074369 ) ) ;
#222 = CARTESIAN_POINT ( 'NONE',  ( -3.636496289402152637, 24.33000000000001961, -11.19198476289190936 ) ) ;
#223 = ORIENTED_EDGE ( 'NONE', *, *, #9601, .T. ) ;
#224 = CARTESIAN_POINT ( 'NONE',  ( -5.623820243337235958, 62.47578838716487581, 12.27284524967300605 ) ) ;
#225 = VERTEX_POINT ( 'NONE', #3915 ) ;
#226 = CARTESIAN_POINT ( 'NONE',  ( -13.39469296682190347, 40.86889263995428934, -1.754359878167341513 ) ) ;
#227 = CARTESIAN_POINT ( 'NONE',  ( -18.62500000000064659, -16.61562499999998010, 7.714727599197333419 ) ) ;
#228 = CARTESIAN_POINT ( 'NONE',  ( -12.06034990428044118, 44.15344642025849708, 6.066424416400918673 ) ) ;
#229 = CARTESIAN_POINT ( 'NONE',  ( -9.831838144771234411, 8.007813437504038845, 15.31996850146883382 ) ) ;
#230 = CARTESIAN_POINT ( 'NONE',  ( -8.691771469529815392E-16, 38.67999999999999972, 14.19474002721660355 ) ) ;
#231 = CARTESIAN_POINT ( 'NONE',  ( 4.171729424061791924, 45.03000000000000114, -12.83926296998457239 ) ) ;
#232 = CARTESIAN_POINT ( 'NONE',  ( -13.49234022047965809, 70.91385223794031845, -0.4697109487732297195 ) ) ;
#233 = CARTESIAN_POINT ( 'NONE',  ( -7.714727599197334307, -64.55312499999983800, -18.62500000000064659 ) ) ;
#234 = CARTESIAN_POINT ( 'NONE',  ( -11.77082077961090967, 67.68472015259277441, -6.610832368286345684 ) ) ;
#235 = CARTESIAN_POINT ( 'NONE',  ( 18.62499999999935341, -58.30937499999983231, 7.714727599200469577 ) ) ;
#236 = CARTESIAN_POINT ( 'NONE',  ( 10.59104740856127513, 54.74884203901541468, -8.371597748919196391 ) ) ;
#237 = EDGE_CURVE ( 'NONE', #1377, #15607, #758, .T. ) ;
#238 = CARTESIAN_POINT ( 'NONE',  ( -3.290095754100384351, 64.29827642083250794, -13.09294913094749191 ) ) ;
#239 = ORIENTED_EDGE ( 'NONE', *, *, #2811, .F. ) ;
#240 = CARTESIAN_POINT ( 'NONE',  ( -4.171729424061791036, 64.53000000000000114, 12.83926296998457239 ) ) ;
#241 = CARTESIAN_POINT ( 'NONE',  ( -12.55115401018059451, 35.11056623410730992, 4.971969969848257342 ) ) ;
#242 = VECTOR ( 'NONE', #6179, 1000.000000000000000 ) ;
#243 = ORIENTED_EDGE ( 'NONE', *, *, #10979, .T. ) ;
#244 = CARTESIAN_POINT ( 'NONE',  ( 13.49341015684798428, 78.44682598755416336, -0.4906469715254504482 ) ) ;
#245 = CARTESIAN_POINT ( 'NONE',  ( 4.171729424061789260, 49.82999999999999829, 12.83926296998457417 ) ) ;
#246 = CARTESIAN_POINT ( 'NONE',  ( 7.500000000000001776, -24.45288220904212295, 8.693347190813737413 ) ) ;
#247 = CARTESIAN_POINT ( 'NONE',  ( 4.352178298388634126, 73.02340726775082658, -12.78109873716751466 ) ) ;
#248 = FACE_OUTER_BOUND ( 'NONE', #11679, .T. ) ;
#249 = CARTESIAN_POINT ( 'NONE',  ( 8.343458848123578520, -14.02000000000000135, 11.48378591275254124 ) ) ;
#250 = CARTESIAN_POINT ( 'NONE',  ( -8.343458848123582072, 68.38000000000000966, 11.48378591275254124 ) ) ;
#251 = CARTESIAN_POINT ( 'NONE',  ( -11.21331758585850302, 52.64752326776081048, -7.517415214335143148 ) ) ;
#252 = CARTESIAN_POINT ( 'NONE',  ( -11.76794919243112325, 45.07999999999999829, 3.823638476888994386 ) ) ;
#253 = CARTESIAN_POINT ( 'NONE',  ( -13.50000000000000000, 63.92999999999999972, -3.306546357697853733E-15 ) ) ;
#254 = CARTESIAN_POINT ( 'NONE',  ( -15.32106749056504569, 7.956441901775577641, -10.18076046065011475 ) ) ;
#255 = AXIS2_PLACEMENT_3D ( 'NONE', #5203, #1206, #13232 ) ;
#256 = CARTESIAN_POINT ( 'NONE',  ( 5.092513312360757105, 68.86389884904878045, 12.50266640507283000 ) ) ;
#257 = CARTESIAN_POINT ( 'NONE',  ( 18.62500000000064304, -1.040624999999997469, -7.714727599197335195 ) ) ;
#258 = CARTESIAN_POINT ( 'NONE',  ( -13.16986379959834252, -63.44374999999986642, -13.16986379960055409 ) ) ;
#259 = CARTESIAN_POINT ( 'NONE',  ( -11.29815970959385041, 74.20716711713330938, 7.389293316686909030 ) ) ;
#260 = CARTESIAN_POINT ( 'NONE',  ( -12.61936853585583940, 76.75616687913201019, -4.797075133751028453 ) ) ;
#261 = CARTESIAN_POINT ( 'NONE',  ( -1.157795017994400766, 7.956106560002618622, -18.35996578475040764 ) ) ;
#262 = CARTESIAN_POINT ( 'NONE',  ( -1.900613283894436512, 1.469143981464172022, 12.00000000000000000 ) ) ;
#263 = CARTESIAN_POINT ( 'NONE',  ( 0.000000000000000000, 9.000000000000000000, 0.000000000000000000 ) ) ;
#264 = SURFACE_SIDE_STYLE ('',( #13938 ) ) ;
#265 = CARTESIAN_POINT ( 'NONE',  ( 2.279995255611139653E-15, -2.819999999999999840, -12.37355403259654985 ) ) ;
#266 = CARTESIAN_POINT ( 'NONE',  ( -11.76794919243112325, 47.77999999999999403, -3.823638476888998827 ) ) ;
#267 = CARTESIAN_POINT ( 'NONE',  ( -13.49999999999999822, 2.079999999999998295, 4.386415899144235020 ) ) ;
#268 = CARTESIAN_POINT ( 'NONE',  ( 4.171729424061789260, 34.82999999999999829, 12.83926296998457417 ) ) ;
#269 = CARTESIAN_POINT ( 'NONE',  ( 13.50148544713888299, 75.42278577149087937, 0.2035154836122704258 ) ) ;
#270 = CARTESIAN_POINT ( 'NONE',  ( 6.243927796512803496, 3.911145512478821826E-16, -15.59435523311979743 ) ) ;
#271 = CARTESIAN_POINT ( 'NONE',  ( -12.43921031607001559, 41.12117747016043978, 5.245971347666045226 ) ) ;
#272 = CARTESIAN_POINT ( 'NONE',  ( 1.218593159756304667, 52.13618204610553875, -13.44511257352553812 ) ) ;
#273 = CARTESIAN_POINT ( 'NONE',  ( 12.50000000000000000, -18.00000000000000355, -2.204364238465235822E-15 ) ) ;
#274 = CARTESIAN_POINT ( 'NONE',  ( 8.248366389433876122, 36.86592902745724132, -10.68712329661759775 ) ) ;
#275 = CYLINDRICAL_SURFACE ( 'NONE', #15212, 13.50000000000000000 ) ;
#276 = DIRECTION ( 'NONE',  ( 0.000000000000000000, -1.000000000000000000, 0.000000000000000000 ) ) ;
#277 = EDGE_CURVE ( 'NONE', #106, #16538, #15358, .T. ) ;
#278 = CARTESIAN_POINT ( 'NONE',  ( -13.41492977785779850, 49.87660617796947093, -1.535378149569272654 ) ) ;
#279 = CARTESIAN_POINT ( 'NONE',  ( 10.79904798291853396, 63.12286850203628319, 8.103746682478284669 ) ) ;
#280 = CARTESIAN_POINT ( 'NONE',  ( 13.31859340417926241, 42.35255605562811354, 2.205733818516509182 ) ) ;
#281 = CARTESIAN_POINT ( 'NONE',  ( 0.4450114281468046107, 38.69606526914740385, 13.49999999987193888 ) ) ;
#282 = ORIENTED_EDGE ( 'NONE', *, *, #13910, .F. ) ;
#283 = CARTESIAN_POINT ( 'NONE',  ( 3.636496289402154414, 72.83000000000001251, 11.19198476289190936 ) ) ;
#284 = CARTESIAN_POINT ( 'NONE',  ( -3.533847551473688675, 70.30706370493864199, -13.03589947523510340 ) ) ;
#285 = CARTESIAN_POINT ( 'NONE',  ( -12.50000000000000000, 98.93000000000002103, -8.999999999999996447 ) ) ;
#286 = ORIENTED_EDGE ( 'NONE', *, *, #1923, .T. ) ;
#287 = CARTESIAN_POINT ( 'NONE',  ( -11.15159978092055937, 43.64371703910293832, -7.608695226596760897 ) ) ;
#288 = CARTESIAN_POINT ( 'NONE',  ( -7.500000000000000000, 106.2138518220599650, -8.084116494856630197 ) ) ;
#289 = CARTESIAN_POINT ( 'NONE',  ( 10.55235452259542051, 60.75099516396964106, -8.420101235079211932 ) ) ;
#290 = CARTESIAN_POINT ( 'NONE',  ( 13.50000000000000000, 4.430000000000003268, 1.734723475976807094E-15 ) ) ;
#291 = CARTESIAN_POINT ( 'NONE',  ( -7.379696451821980833E-14, 6.046025403784444308, -12.00000000000000000 ) ) ;
#292 = CARTESIAN_POINT ( 'NONE',  ( 13.45831588147710178, 66.39312768838394163, 1.061907957825456883 ) ) ;
#293 = CARTESIAN_POINT ( 'NONE',  ( 10.60402044222889373, 57.11187693063078541, 8.355290479010609062 ) ) ;
#294 = CARTESIAN_POINT ( 'NONE',  ( -3.636496289402153081, 56.32999999999999829, -11.19198476289190936 ) ) ;
#295 = CARTESIAN_POINT ( 'NONE',  ( 11.76794919243112325, 64.28000000000000114, 3.823638476888996607 ) ) ;
#296 = CARTESIAN_POINT ( 'NONE',  ( -12.44014281442525949, 47.12117745437350180, 5.246275075209847927 ) ) ;
#297 = CARTESIAN_POINT ( 'NONE',  ( 5.553566080697077467, 45.97850270378070547, -12.30479239002528935 ) ) ;
#298 = CARTESIAN_POINT ( 'NONE',  ( 12.00000000000006217, 8.563974596215590651, 1.734723475976807094E-15 ) ) ;
#299 = CARTESIAN_POINT ( 'NONE',  ( 0.2547235083979552117, 31.17084125670657357, -13.49760154729842476 ) ) ;
#300 = CARTESIAN_POINT ( 'NONE',  ( -5.563626996627561994, 56.47811886027594142, 12.30024710206874694 ) ) ;
#301 = CARTESIAN_POINT ( 'NONE',  ( 4.711679271993006068, -46.82812499999989342, 11.37500000000039257 ) ) ;
#302 = CARTESIAN_POINT ( 'NONE',  ( -13.50000000000000000, 51.93000000000000682, -3.306546357697853733E-15 ) ) ;
#303 = VECTOR ( 'NONE', #7629, 1000.000000000000000 ) ;
#304 = CARTESIAN_POINT ( 'NONE',  ( 1.276060874233202469, 32.72588244700077098, 13.43956583305223873 ) ) ;
#305 = CARTESIAN_POINT ( 'NONE',  ( -17.42428528562830792, 5.918584287042170544, -19.29752010712871169 ) ) ;
#306 = CARTESIAN_POINT ( 'NONE',  ( 4.086892649892674534, 40.03309646582929560, -12.86683993615205424 ) ) ;
#307 = ORIENTED_EDGE ( 'NONE', *, *, #8201, .F. ) ;
#308 = CARTESIAN_POINT ( 'NONE',  ( -5.300476046473269420, 62.48820044638870996, 12.41629279154124710 ) ) ;
#309 = VERTEX_POINT ( 'NONE', #1472 ) ;
#310 = CARTESIAN_POINT ( 'NONE',  ( -13.46982610043145812, 40.96195804405107310, 0.9247321941779073073 ) ) ;
#311 = CARTESIAN_POINT ( 'NONE',  ( 7.714727599197340524, -70.72812499999984936, 18.62500000000063949 ) ) ;
#312 = CARTESIAN_POINT ( 'NONE',  ( -13.49104613329688007, 43.91131453512677751, -0.5374766152377549178 ) ) ;
#313 = CARTESIAN_POINT ( 'NONE',  ( 13.50000000000000355, 65.57999999999998408, -4.386415899144233244 ) ) ;
#314 = CARTESIAN_POINT ( 'NONE',  ( 4.171729424061791924, 31.02999999999999403, -12.83926296998457239 ) ) ;
#315 = CARTESIAN_POINT ( 'NONE',  ( 4.171729424061791924, 48.02999999999999403, -12.83926296998457239 ) ) ;
#316 = CARTESIAN_POINT ( 'NONE',  ( -9.629907599157546016, 46.56016663611932671, -9.461235684485890474 ) ) ;
#317 = CARTESIAN_POINT ( 'NONE',  ( -11.63915563610238735, 67.67541942150826628, -6.840021065327532845 ) ) ;
#318 = CARTESIAN_POINT ( 'NONE',  ( 13.16986379959833897, -73.91874999999977547, 13.16986379960055409 ) ) ;
#319 = EDGE_CURVE ( 'NONE', #9628, #17318, #5798, .T. ) ;
#320 = CARTESIAN_POINT ( 'NONE',  ( 12.41362727660819409, 54.23603978842571394, 5.323407497928233312 ) ) ;
#321 = CARTESIAN_POINT ( 'NONE',  ( -4.350728866308207543, 64.33618153779571003, -12.78724907277022282 ) ) ;
#322 = ORIENTED_EDGE ( 'NONE', *, *, #15118, .T. ) ;
#323 = CARTESIAN_POINT ( 'NONE',  ( -8.343458848123582072, 64.37999999999998124, 11.48378591275253768 ) ) ;
#324 = CARTESIAN_POINT ( 'NONE',  ( -13.25540151110283915, 35.02074204735390595, 2.572278351385800743 ) ) ;
#325 = ORIENTED_EDGE ( 'NONE', *, *, #12398, .T. ) ;
#326 = CARTESIAN_POINT ( 'NONE',  ( 12.90178577204087063, 78.28740904515449017, 3.975375597352175383 ) ) ;
#327 = CARTESIAN_POINT ( 'NONE',  ( -7.500000000000000000, 98.93000000000002103, 1.224646799147353059E-15 ) ) ;
#328 = CARTESIAN_POINT ( 'NONE',  ( -8.891200544363830713E-16, 37.67999999999999261, 13.50000000000000000 ) ) ;
#329 = CARTESIAN_POINT ( 'NONE',  ( 11.03100386637765595, 72.72352357107607190, -7.783825102783979766 ) ) ;
#330 = CARTESIAN_POINT ( 'NONE',  ( 2.306785515682943544, 79.09706103861046245, -13.30169983709586035 ) ) ;
#331 = CARTESIAN_POINT ( 'NONE',  ( 8.343458848123578520, -17.01999999999999957, 11.48378591275254124 ) ) ;
#332 = CARTESIAN_POINT ( 'NONE',  ( 13.50000000000000000, 63.42999999999999972, 1.653273178848926867E-15 ) ) ;
#333 = CARTESIAN_POINT ( 'NONE',  ( -13.45789989295631983, 52.96690304976064567, 1.065472127645539890 ) ) ;
#334 = CARTESIAN_POINT ( 'NONE',  ( 7.272992578804308828, 39.97999999999999687, 10.01041549318726709 ) ) ;
#335 = CARTESIAN_POINT ( 'NONE',  ( 7.272992578804311492, -18.12000000000000455, -10.01041549318726709 ) ) ;
#336 = CARTESIAN_POINT ( 'NONE',  ( 4.171729424061791924, 60.03000000000000114, -12.83926296998457239 ) ) ;
#337 = CARTESIAN_POINT ( 'NONE',  ( -8.891200544363830713E-16, 34.67999999999999261, 13.50000000000000000 ) ) ;
#338 = CARTESIAN_POINT ( 'NONE',  ( 5.057394672961640580, 68.86257603500035884, 12.51691328543133785 ) ) ;
#339 = CARTESIAN_POINT ( 'NONE',  ( 0.000000000000000000, -1.200000000000000030E-05, 0.000000000000000000 ) ) ;
#340 = FACE_OUTER_BOUND ( 'NONE', #15456, .T. ) ;
#341 = CARTESIAN_POINT ( 'NONE',  ( 13.16986379960055409, -75.93124999999983515, -13.16986379959834430 ) ) ;
#342 = CARTESIAN_POINT ( 'NONE',  ( -12.53724792357792417, 74.11243421711593271, 5.024370009789406843 ) ) ;
#343 = CARTESIAN_POINT ( 'NONE',  ( -6.452387276988709175, 76.41704375434667895, -11.86051681251366574 ) ) ;
#344 = DIRECTION ( 'NONE',  ( 0.000000000000000000, -1.000000000000000000, 0.000000000000000000 ) ) ;
#345 = CARTESIAN_POINT ( 'NONE',  ( 12.50000000000000000, 98.93000000000002103, 9.000000000000000000 ) ) ;
#346 = DIRECTION ( 'NONE',  ( 0.000000000000000000, -1.000000000000000000, 0.000000000000000000 ) ) ;
#347 = FACE_OUTER_BOUND ( 'NONE', #6188, .T. ) ;
#348 = CARTESIAN_POINT ( 'NONE',  ( 11.76794919243112680, -9.419999999999999929, -3.823638476888993942 ) ) ;
#349 = CARTESIAN_POINT ( 'NONE',  ( -9.520470885617717371, 33.22999999999999687, 6.917026985038133624 ) ) ;
#350 = AXIS2_PLACEMENT_3D ( 'NONE', #8881, #10118, #2121 ) ;
#351 = CARTESIAN_POINT ( 'NONE',  ( -9.367636073990613710, 32.31297664171835038, 9.721046613647347456 ) ) ;
#352 = B_SPLINE_CURVE_WITH_KNOTS ( 'NONE', 3,
 ( #3485, #13293, #14513, #4996 ),
 .UNSPECIFIED., .F., .F.,
 ( 4, 4 ),
 ( 2.383248697869603246E-07, 0.007646667935218606771 ),
 .UNSPECIFIED. ) ;
#353 = CARTESIAN_POINT ( 'NONE',  ( 11.98090966731797913, 75.20012104151170718, 6.225558393635502341 ) ) ;
#354 = CARTESIAN_POINT ( 'NONE',  ( 8.083740994923175549, 5.967892910702088472E-16, -9.063702410685676725 ) ) ;
#355 = ADVANCED_FACE ( 'NONE', ( #5565 ), #16407, .F. ) ;
#356 = CARTESIAN_POINT ( 'NONE',  ( 5.883989548015875926, 30.92926152634062475, 10.19133431864935879 ) ) ;
#357 = CARTESIAN_POINT ( 'NONE',  ( 4.171729424061791924, 84.03000000000000114, -12.83926296998457239 ) ) ;
#358 = CARTESIAN_POINT ( 'NONE',  ( 4.717239269204677399, 52.01011083281174052, -12.64902143884823893 ) ) ;
#359 = FACE_OUTER_BOUND ( 'NONE', #797, .T. ) ;
#360 = AXIS2_PLACEMENT_3D ( 'NONE', #566, #14158, #6227 ) ;
#361 = DIRECTION ( 'NONE',  ( 0.000000000000000000, 0.000000000000000000, 1.000000000000000000 ) ) ;
#362 = CARTESIAN_POINT ( 'NONE',  ( -7.416407864998753041, 0.6139745962155744863, -10.20780970022450340 ) ) ;
#363 = FACE_OUTER_BOUND ( 'NONE', #6334, .T. ) ;
#364 = CARTESIAN_POINT ( 'NONE',  ( 9.731717852235492572, 63.06533615564348594, 9.356802677010852776 ) ) ;
#365 = CARTESIAN_POINT ( 'NONE',  ( 13.41797430850394690, 42.37741962985320043, 1.511824690427647111 ) ) ;
#366 = CARTESIAN_POINT ( 'NONE',  ( 6.007520941189540054, 48.96077821041167510, -12.08973124302788449 ) ) ;
#367 = CARTESIAN_POINT ( 'NONE',  ( 3.636496289402157078, 21.02999999999999403, -11.19198476289190936 ) ) ;
#368 = VERTEX_POINT ( 'NONE', #6709 ) ;
#369 = CARTESIAN_POINT ( 'NONE',  ( -7.272992578804310604, 78.38000000000000966, 10.01041549318726886 ) ) ;
#370 = FACE_OUTER_BOUND ( 'NONE', #4288, .T. ) ;
#371 = CARTESIAN_POINT ( 'NONE',  ( 11.37500000000039435, -67.64062499999984368, -4.711679271993003404 ) ) ;
#372 = CARTESIAN_POINT ( 'NONE',  ( 2.621994543952811015E-15, 4.180000000000005045, -14.19474002721660355 ) ) ;
#373 = ORIENTED_EDGE ( 'NONE', *, *, #8679, .F. ) ;
#374 = CARTESIAN_POINT ( 'NONE',  ( -7.499999999999998224, 106.0143933292129503, -8.253836299850743075 ) ) ;
#375 = CARTESIAN_POINT ( 'NONE',  ( 13.37389533385238671, 60.49657913131436970, -1.904068468163566230 ) ) ;
#376 = CARTESIAN_POINT ( 'NONE',  ( -13.49999999999999822, 6.080000000000002736, 4.386415899144235908 ) ) ;
#377 = CARTESIAN_POINT ( 'NONE',  ( 1.900613283881106952, 0.2370931738958342305, -12.00000000000433253 ) ) ;
#378 = CARTESIAN_POINT ( 'NONE',  ( 17.32050807568878170, 0.000000000000000000, -7.999999999999961808 ) ) ;
#379 = CARTESIAN_POINT ( 'NONE',  ( 11.37538673181245130, 66.15763038601566848, 7.273122068539749741 ) ) ;
#380 = CARTESIAN_POINT ( 'NONE',  ( 2.785878927130813844E-06, 56.68007738487546732, 13.49999999999942979 ) ) ;
#381 = EDGE_CURVE ( 'NONE', #2740, #4566, #8901, .T. ) ;
#382 = CARTESIAN_POINT ( 'NONE',  ( 7.272992578804308828, 57.97999999999999687, 10.01041549318726709 ) ) ;
#383 = CARTESIAN_POINT ( 'NONE',  ( 13.49999999999999822, 35.28000000000000114, 4.386415899144237684 ) ) ;
#384 = CARTESIAN_POINT ( 'NONE',  ( 2.272985001014427788E-15, 71.17999999999999261, -12.37355403259654985 ) ) ;
#385 = CARTESIAN_POINT ( 'NONE',  ( -12.57369232349585175, 46.75164900414807789, -4.914502090225122188 ) ) ;
#386 = CARTESIAN_POINT ( 'NONE',  ( 6.864326658960421490, 45.92603133891358169, -11.62547684485642030 ) ) ;
#387 = CARTESIAN_POINT ( 'NONE',  ( 1.296431213746159106, 7.924856485849745447, -18.46737842244078465 ) ) ;
#388 = CARTESIAN_POINT ( 'NONE',  ( 5.441320307982408622, 30.98247815750375977, -12.35517929490900535 ) ) ;
#389 = CARTESIAN_POINT ( 'NONE',  ( -5.530913952003127854, 56.47938171940309360, 12.31500263983988397 ) ) ;
#390 = CARTESIAN_POINT ( 'NONE',  ( -8.043339635997654113, -77.00624999999982379, 8.043339635996302306 ) ) ;
#391 = CARTESIAN_POINT ( 'NONE',  ( -3.715634683528351356, 50.54639745666956685, 12.97889439479828688 ) ) ;
#392 = FACE_OUTER_BOUND ( 'NONE', #17425, .T. ) ;
#393 = CARTESIAN_POINT ( 'NONE',  ( -17.42428528562830436, 0.000000000000000000, -19.29752010712870813 ) ) ;
#394 = CARTESIAN_POINT ( 'NONE',  ( -7.999999999999776179, 7.773118517290098062, -17.32050807568887762 ) ) ;
#395 = EDGE_LOOP ( 'NONE', ( #15239, #541, #10576, #13529, #15146, #9172, #16089, #3558, #4390, #13299, #1334, #7181, #3213, #17164, #13126, #14247, #17014, #6081, #7599, #5297, #13812, #9329, #10126, #2086, #12913, #1173, #1080, #16108, #1978 ) ) ;
#396 = CARTESIAN_POINT ( 'NONE',  ( -13.46679717695066003, 61.96273041894593803, 0.9463406209475275777 ) ) ;
#397 = EDGE_LOOP ( 'NONE', ( #3454, #14162, #14933, #4128 ) ) ;
#398 = CARTESIAN_POINT ( 'NONE',  ( 11.76794919243112325, -15.71999999999999709, 3.823638476888996163 ) ) ;
#399 = CARTESIAN_POINT ( 'NONE',  ( -13.16986379959834252, -63.44374999999986642, -13.16986379960055409 ) ) ;
#400 = CARTESIAN_POINT ( 'NONE',  ( -12.76959190857851212, 43.77205537680598724, -4.381403554202501383 ) ) ;
#401 = CARTESIAN_POINT ( 'NONE',  ( -8.349340579021736986, 8.007293667506184320, 16.17792858571905157 ) ) ;
#402 = CARTESIAN_POINT ( 'NONE',  ( -13.49999999999999822, 37.77999999999998693, -4.386415899144240349 ) ) ;
#403 = CARTESIAN_POINT ( 'NONE',  ( -8.343458848123576743, 45.47999999999998977, -11.48378591275254301 ) ) ;
#404 = ADVANCED_FACE ( 'NONE', ( #4042 ), #9457, .T. ) ;
#405 = CARTESIAN_POINT ( 'NONE',  ( -1.743841339441459137, 46.24267996541158965, -13.38863380285367910 ) ) ;
#406 = CARTESIAN_POINT ( 'NONE',  ( -5.259139341736429607, 67.37018746444084627, -12.43396276512746823 ) ) ;
#407 = CARTESIAN_POINT ( 'NONE',  ( 13.16986379959833897, -57.26874999999984794, 13.16986379960055409 ) ) ;
#408 = CARTESIAN_POINT ( 'NONE',  ( 3.272540978394824940, 53.79766787922819304, 13.09734638618094138 ) ) ;
#409 = CARTESIAN_POINT ( 'NONE',  ( -2.209888104562151234, 64.25951276812958213, -13.32892421627443724 ) ) ;
#410 = ORIENTED_EDGE ( 'NONE', *, *, #17256, .F. ) ;
#411 = CARTESIAN_POINT ( 'NONE',  ( -8.111752993934361555, 34.48789724560310788, -10.79119880849037472 ) ) ;
#412 = CARTESIAN_POINT ( 'NONE',  ( 11.37500000000039435, -17.69062499999995453, -4.711679271993004292 ) ) ;
#413 = CARTESIAN_POINT ( 'NONE',  ( 13.45153961929852748, 78.46975942807824822, -1.146847328308098879 ) ) ;
#414 = CARTESIAN_POINT ( 'NONE',  ( -15.34527529650339872, 7.924527530346060722, 10.35822530491739535 ) ) ;
#415 = CARTESIAN_POINT ( 'NONE',  ( 2.207926304393408011E-15, 8.062177826491096155, 17.99999999999999645 ) ) ;
#416 = VECTOR ( 'NONE', #15327, 1000.000000000000000 ) ;
#417 = CARTESIAN_POINT ( 'NONE',  ( 7.500000000000002665, -26.57032277106731755, -6.479247348114214766 ) ) ;
#418 = CARTESIAN_POINT ( 'NONE',  ( 13.42160645633606286, 72.48917881215648151, -1.700578753849256941 ) ) ;
#419 = CARTESIAN_POINT ( 'NONE',  ( -11.76794919243112325, 33.93000000000001393, -2.602085213965210642E-15 ) ) ;
#420 = CARTESIAN_POINT ( 'NONE',  ( -4.171729424061787483, 58.32999999999999829, -12.83926296998457417 ) ) ;
#421 = CARTESIAN_POINT ( 'NONE',  ( -13.46160622163430176, 52.96521979142928416, 1.017449871812443618 ) ) ;
#422 = EDGE_CURVE ( 'NONE', #9696, #11984, #11941, .T. ) ;
#423 = CARTESIAN_POINT ( 'NONE',  ( 3.636496289402154414, 39.82999999999999829, 11.19198476289190936 ) ) ;
#424 = CARTESIAN_POINT ( 'NONE',  ( 11.76794919243112325, -18.72000000000000952, 3.823638476888996163 ) ) ;
#425 = CARTESIAN_POINT ( 'NONE',  ( 8.343458848123578520, 55.97999999999998977, 11.48378591275254124 ) ) ;
#426 = CARTESIAN_POINT ( 'NONE',  ( 1.511718349539964201, 50.73435581608389100, 13.41509433142833885 ) ) ;
#427 = CARTESIAN_POINT ( 'NONE',  ( -3.636496289402152637, 0.3299999999999969624, -11.19198476289190936 ) ) ;
#428 = CARTESIAN_POINT ( 'NONE',  ( 4.442947237195123300, 68.83971558705859195, 12.75121963132532343 ) ) ;
#429 = CARTESIAN_POINT ( 'NONE',  ( 9.708203932499388955, 2.263974596215569512, 7.053423027509694521 ) ) ;
#430 = DIRECTION ( 'NONE',  ( 0.000000000000000000, 0.000000000000000000, -1.000000000000000000 ) ) ;
#431 = CARTESIAN_POINT ( 'NONE',  ( 13.16986379960055409, -92.58124999999979821, -13.16986379959834430 ) ) ;
#432 = CARTESIAN_POINT ( 'NONE',  ( -13.33044600843074612, 73.85509119750386731, -2.135332589583271545 ) ) ;
#433 = CARTESIAN_POINT ( 'NONE',  ( -2.187775580252431684, 76.25866090160262445, -13.32182888840495139 ) ) ;
#434 = DIRECTION ( 'NONE',  ( 1.000000000000000000, 0.000000000000000000, 0.000000000000000000 ) ) ;
#435 = DIRECTION ( 'NONE',  ( 0.000000000000000000, 0.000000000000000000, -1.000000000000000000 ) ) ;
#436 = CARTESIAN_POINT ( 'NONE',  ( -10.92172942406179104, 30.23000000000000753, 7.935100905948385908 ) ) ;
#437 = CARTESIAN_POINT ( 'NONE',  ( 9.520470885617715595, -9.869999999999997442, 6.917026985038135400 ) ) ;
#438 = CARTESIAN_POINT ( 'NONE',  ( 11.76794919243112325, 34.28000000000000114, 3.823638476888997051 ) ) ;
#439 = CARTESIAN_POINT ( 'NONE',  ( 13.50000000000000000, -17.56999999999999673, 1.734723475976807094E-15 ) ) ;
#440 = CARTESIAN_POINT ( 'NONE',  ( -1.636861439990225930, 32.62114992449928508, 13.40040588940331112 ) ) ;
#441 = CARTESIAN_POINT ( 'NONE',  ( 1.678346760273044636, 74.74034482231108711, 13.39582455766600866 ) ) ;
#442 = CARTESIAN_POINT ( 'NONE',  ( 3.195015426203765330, 7.495012466571534215E-16, -14.06913727495813937 ) ) ;
#443 = CARTESIAN_POINT ( 'NONE',  ( -9.520470885617715595, 32.63000000000000256, -6.917026985038136289 ) ) ;
#444 = CARTESIAN_POINT ( 'NONE',  ( -13.49999999999999822, 84.78000000000001535, -4.386415899144240349 ) ) ;
#445 = CARTESIAN_POINT ( 'NONE',  ( 10.26872965863894471, 51.76653688478288018, -8.764966814524187910 ) ) ;
#446 = VECTOR ( 'NONE', #7079, 1000.000000000000000 ) ;
#447 = CARTESIAN_POINT ( 'NONE',  ( -5.433831064015286927, 38.48323282879334073, 12.36477467734148483 ) ) ;
#448 = CARTESIAN_POINT ( 'NONE',  ( 5.755010883477707395, 36.97068350995541408, -12.21187340796739207 ) ) ;
#449 = FACE_OUTER_BOUND ( 'NONE', #15937, .T. ) ;
#450 = CYLINDRICAL_SURFACE ( 'NONE', #1302, 1.999999999999998224 ) ;
#451 = CARTESIAN_POINT ( 'NONE',  ( 6.814633543800678872, 62.93188781794702180, 11.65614756620777115 ) ) ;
#452 = CARTESIAN_POINT ( 'NONE',  ( 13.47189594166342097, 42.46064207325136408, -0.8869200912900612188 ) ) ;
#453 = CARTESIAN_POINT ( 'NONE',  ( 10.86073516050613641, 48.73349978075351885, -8.018644299739561276 ) ) ;
#454 = CARTESIAN_POINT ( 'NONE',  ( -3.636496289402156190, 19.53000000000001890, 11.19198476289190758 ) ) ;
#455 = ADVANCED_FACE ( 'NONE', ( #248 ), #1382, .T. ) ;
#456 = ORIENTED_EDGE ( 'NONE', *, *, #3724, .T. ) ;
#457 = CARTESIAN_POINT ( 'NONE',  ( 7.272992578804308828, 66.98000000000000398, 10.01041549318726886 ) ) ;
#458 = CARTESIAN_POINT ( 'NONE',  ( 18.62499999999935341, -91.60937499999975842, 7.714727599200469577 ) ) ;
#459 = CARTESIAN_POINT ( 'NONE',  ( -8.043339635997654113, -43.70624999999989768, 8.043339635996302306 ) ) ;
#460 = CARTESIAN_POINT ( 'NONE',  ( 8.343458848123583849, 3.879999999999999449, -11.48378591275253768 ) ) ;
#461 = EDGE_LOOP ( 'NONE', ( #13360, #12852 ) ) ;
#462 = CARTESIAN_POINT ( 'NONE',  ( -7.409984580736203970E-16, 28.67999999999999972, 12.37355403259654985 ) ) ;
#463 = FACE_OUTER_BOUND ( 'NONE', #11574, .T. ) ;
#464 = PRESENTATION_LAYER_ASSIGNMENT (  '', '', ( #8657 ) ) ;
#465 = CARTESIAN_POINT ( 'NONE',  ( -4.171729424061787483, -0.6700000000000039257, -12.83926296998457417 ) ) ;
#466 = CARTESIAN_POINT ( 'NONE',  ( -1.564113515457998572E-12, -12.48749999999997051, 18.62500000000000000 ) ) ;
#467 = CARTESIAN_POINT ( 'NONE',  ( 12.56982549204153976, 66.25104303858046251, 4.931975050715497133 ) ) ;
#468 = CARTESIAN_POINT ( 'NONE',  ( 0.4447238818697385465, 56.69608407970753206, 13.49999999965100805 ) ) ;
#469 = CARTESIAN_POINT ( 'NONE',  ( -9.520470885617717371, 57.23000000000000398, 6.917026985038133624 ) ) ;
#470 = CARTESIAN_POINT ( 'NONE',  ( -7.272992578804307939, 65.48000000000000398, -10.01041549318726886 ) ) ;
#471 = CARTESIAN_POINT ( 'NONE',  ( -13.45448328032910901, 46.96959999993933366, 1.138838731259335768 ) ) ;
#472 = CARTESIAN_POINT ( 'NONE',  ( 9.149453984131964646, 45.82364388978120928, -9.926606263152381260 ) ) ;
#473 = CARTESIAN_POINT ( 'NONE',  ( 4.340711467061829865, 70.02384940047436146, -12.81345992402683365 ) ) ;
#474 = CARTESIAN_POINT ( 'NONE',  ( -8.000000000000197176, 0.000000000000000000, 24.73863375370590134 ) ) ;
#475 = CARTESIAN_POINT ( 'NONE',  ( 10.77555668018642976, 30.73860136405477661, -8.141750913204777618 ) ) ;
#476 = CARTESIAN_POINT ( 'NONE',  ( -11.61452348585071803, 10.00000000000000000, -3.545951533830508762 ) ) ;
#477 = CARTESIAN_POINT ( 'NONE',  ( -3.318711775807452913, 50.56063369891364800, 13.08625922055076174 ) ) ;
#478 = CARTESIAN_POINT ( 'NONE',  ( 12.85438585762840091, 33.28169117570074320, 4.130889853976885462 ) ) ;
#479 = CARTESIAN_POINT ( 'NONE',  ( -1.747636201723826943, 10.00000000000000000, 12.72100980577129015 ) ) ;
#480 = FACE_OUTER_BOUND ( 'NONE', #14679, .T. ) ;
#481 = CARTESIAN_POINT ( 'NONE',  ( 9.520470885617717371, 23.73000000000000043, -6.917026985038131848 ) ) ;
#482 = EDGE_CURVE ( 'NONE', #6493, #2917, #12344, .T. ) ;
#483 = EDGE_LOOP ( 'NONE', ( #13081, #14244, #14288, #13557 ) ) ;
#484 = CARTESIAN_POINT ( 'NONE',  ( -12.86035813447160514, 62.07770165908708293, 4.111105408976296616 ) ) ;
#485 = ORIENTED_EDGE ( 'NONE', *, *, #139, .F. ) ;
#486 = CARTESIAN_POINT ( 'NONE',  ( 2.279995255611139653E-15, -14.82000000000000384, -12.37355403259654985 ) ) ;
#487 = CARTESIAN_POINT ( 'NONE',  ( 7.714727599197340524, -37.42812499999993037, 18.62500000000063949 ) ) ;
#488 = CARTESIAN_POINT ( 'NONE',  ( 10.82670249703553722, 48.12451974694700141, 8.064369848088544401 ) ) ;
#489 = DIRECTION ( 'NONE',  ( 0.000000000000000000, 1.000000000000000000, 0.000000000000000000 ) ) ;
#490 = CARTESIAN_POINT ( 'NONE',  ( 10.92172942406178926, 33.13000000000000256, 7.935100905948387684 ) ) ;
#491 = CARTESIAN_POINT ( 'NONE',  ( 8.343458848123578520, 40.97999999999998977, 11.48378591275254124 ) ) ;
#492 = CARTESIAN_POINT ( 'NONE',  ( -0.5656080267661869332, 46.20032726311463733, -13.48884909811126676 ) ) ;
#493 = CARTESIAN_POINT ( 'NONE',  ( -11.00247426292009933, 67.63473743967996654, -7.822801183469714204 ) ) ;
#494 = CARTESIAN_POINT ( 'NONE',  ( 1.561832610794586740E-12, -63.51249999999981810, -18.62500000000000000 ) ) ;
#495 = CARTESIAN_POINT ( 'NONE',  ( 9.838722238819098465, 54.07056626371765162, 9.256620450124710686 ) ) ;
#496 = ORIENTED_EDGE ( 'NONE', *, *, #13515, .F. ) ;
#497 = CARTESIAN_POINT ( 'NONE',  ( -2.994742845161742384, 64.28778625662059198, -13.16386178499985782 ) ) ;
#498 = EDGE_CURVE ( 'NONE', #15482, #11876, #15501, .T. ) ;
#499 = ORIENTED_EDGE ( 'NONE', *, *, #16100, .T. ) ;
#500 = DIRECTION ( 'NONE',  ( 1.000000000000000000, 8.673617379884039170E-17, -0.000000000000000000 ) ) ;
#501 = CARTESIAN_POINT ( 'NONE',  ( -10.71871353429217244, 34.61762525966922510, -8.218939176556370185 ) ) ;
#502 = CARTESIAN_POINT ( 'NONE',  ( -8.043339635996302306, -56.19374999999985931, -8.043339635997654113 ) ) ;
#503 = CARTESIAN_POINT ( 'NONE',  ( 10.91305626273815577, 78.12916640448000294, 7.952299940727153960 ) ) ;
#504 = LINE ( 'NONE', #6976, #14193 ) ;
#505 = CARTESIAN_POINT ( 'NONE',  ( 11.90602345876549073, 72.66532707484691400, -6.363701510510520798 ) ) ;
#506 = CARTESIAN_POINT ( 'NONE',  ( -3.636496289402152637, 30.32999999999999474, -11.19198476289190936 ) ) ;
#507 = CARTESIAN_POINT ( 'NONE',  ( -13.49999999999999822, 59.07999999999999119, 4.386415899144235908 ) ) ;
#508 = CARTESIAN_POINT ( 'NONE',  ( -4.120143485240188141, 52.32813700730908835, -12.85633956262296174 ) ) ;
#509 = CARTESIAN_POINT ( 'NONE',  ( -11.76794919243112325, 35.77999999999999403, -3.823638476888998827 ) ) ;
#510 = CARTESIAN_POINT ( 'NONE',  ( 13.50000000000000355, 59.57999999999999829, -4.386415899144233244 ) ) ;
#511 = CARTESIAN_POINT ( 'NONE',  ( -15.50029318102132336, 8.062211461649205546, -9.152478727637765488 ) ) ;
#512 = CARTESIAN_POINT ( 'NONE',  ( -3.636496289402156190, -4.469999999999994422, 11.19198476289190758 ) ) ;
#513 = CARTESIAN_POINT ( 'NONE',  ( 7.978366338076175346, 68.98190559513436426, 10.89111902590045489 ) ) ;
#514 = DIRECTION ( 'NONE',  ( 0.000000000000000000, 0.000000000000000000, 1.000000000000000000 ) ) ;
#515 = CARTESIAN_POINT ( 'NONE',  ( -8.343458848123578520, 72.48000000000000398, -11.48378591275254124 ) ) ;
#516 = CARTESIAN_POINT ( 'NONE',  ( 18.62500000000064659, -91.54062499999980673, -7.714727599197336083 ) ) ;
#517 = CARTESIAN_POINT ( 'NONE',  ( -11.11816795611437669, 73.64147893977222736, -7.662807821280736675 ) ) ;
#518 = DIRECTION ( 'NONE',  ( -0.5000000000000074385, 0.000000000000000000, 0.8660254037844342667 ) ) ;
#519 = ADVANCED_FACE ( 'NONE', ( #7494 ), #12874, .T. ) ;
#520 = CARTESIAN_POINT ( 'NONE',  ( 3.708203932499371192, 8.896025403784447505, -11.41267819554184548 ) ) ;
#521 = FACE_OUTER_BOUND ( 'NONE', #11792, .T. ) ;
#522 = CARTESIAN_POINT ( 'NONE',  ( -1.245860404445607248E-06, 40.18000018109674443, -13.49999999999994316 ) ) ;
#523 = CARTESIAN_POINT ( 'NONE',  ( 11.76794919243112325, -6.569999999999999396, 1.734723475976807094E-15 ) ) ;
#524 = CARTESIAN_POINT ( 'NONE',  ( 11.76794919243112325, 40.42999999999999972, 1.441158131103945434E-15 ) ) ;
#525 = CARTESIAN_POINT ( 'NONE',  ( -11.27597249832626680, 32.20855542261740823, 7.423102544681950299 ) ) ;
#526 = CARTESIAN_POINT ( 'NONE',  ( 8.989377126757293723, 75.02817402051516638, 10.09332704491346178 ) ) ;
#527 = CARTESIAN_POINT ( 'NONE',  ( 4.171729424061789260, 61.82999999999999829, 12.83926296998457417 ) ) ;
#528 = AXIS2_PLACEMENT_3D ( 'NONE', #15251, #16589, #5659 ) ;
#529 =( LENGTH_UNIT ( ) NAMED_UNIT ( * ) SI_UNIT ( .MILLI., .METRE. ) );
#530 = CARTESIAN_POINT ( 'NONE',  ( -10.92172942406178926, 84.62999999999999545, -7.935100905948389460 ) ) ;
#531 = CARTESIAN_POINT ( 'NONE',  ( 0.9721905075920033168, 52.14504527273197709, -13.46523144585630405 ) ) ;
#532 = CARTESIAN_POINT ( 'NONE',  ( -4.278914508684592555, 38.52614286959915546, 12.80401563806038467 ) ) ;
#533 = CARTESIAN_POINT ( 'NONE',  ( 8.272675178529885542, 36.86482438541639794, -10.66831387527186870 ) ) ;
#534 = DIRECTION ( 'NONE',  ( -3.741588754404567345E-15, 0.000000000000000000, 1.000000000000000000 ) ) ;
#535 = CARTESIAN_POINT ( 'NONE',  ( -1.117795391647952385, 49.22012975758181597, -13.45637554176790474 ) ) ;
#536 = CARTESIAN_POINT ( 'NONE',  ( 11.32484296497576182, 63.15460178810015890, 7.350387779789046228 ) ) ;
#537 = CARTESIAN_POINT ( 'NONE',  ( 1.536173093022593195, 41.73525089061148918, 13.41486744188283353 ) ) ;
#538 = CARTESIAN_POINT ( 'NONE',  ( 7.996676220521883316, 48.87726588079390666, -10.87843020462947408 ) ) ;
#539 = CIRCLE ( 'NONE', #3640, 5.000000000000000000 ) ;
#540 = CARTESIAN_POINT ( 'NONE',  ( 7.272992578804311492, 17.87999999999999190, -10.01041549318726709 ) ) ;
#541 = ORIENTED_EDGE ( 'NONE', *, *, #14987, .T. ) ;
#542 = CARTESIAN_POINT ( 'NONE',  ( -3.636496289402155746, 66.53000000000000114, 11.19198476289190936 ) ) ;
#543 = CARTESIAN_POINT ( 'NONE',  ( -8.043339635997654113, -19.80624999999993463, 8.043339635996304082 ) ) ;
#544 = CARTESIAN_POINT ( 'NONE',  ( 8.043339635997654113, -52.03124999999987921, -8.043339635996304082 ) ) ;
#545 = CARTESIAN_POINT ( 'NONE',  ( -8.343458848123582072, 5.379999999999996341, 11.48378591275254124 ) ) ;
#546 = VERTEX_POINT ( 'NONE', #930 ) ;
#547 = CARTESIAN_POINT ( 'NONE',  ( -8.711848673603300952, 80.92999999999996419, -8.870066681593291591 ) ) ;
#548 = CARTESIAN_POINT ( 'NONE',  ( -4.171729424061791036, 0.5300000000000026912, 12.83926296998457239 ) ) ;
#549 = CYLINDRICAL_SURFACE ( 'NONE', #615, 5.000000000000000000 ) ;
#550 = CARTESIAN_POINT ( 'NONE',  ( 11.01344701655966141, 66.13478396425333017, 7.819520221991368203 ) ) ;
#551 = CARTESIAN_POINT ( 'NONE',  ( 4.171729424061791924, 82.03000000000000114, -12.83926296998457239 ) ) ;
#552 = CARTESIAN_POINT ( 'NONE',  ( 11.76794919243112325, 64.28000000000000114, 3.823638476888996607 ) ) ;
#553 = CARTESIAN_POINT ( 'NONE',  ( 0.2252273365623476686, 31.65984393938649433, 15.45843899586302150 ) ) ;
#554 = CARTESIAN_POINT ( 'NONE',  ( 3.636496289402154414, 60.82999999999999829, 11.19198476289190936 ) ) ;
#555 = CARTESIAN_POINT ( 'NONE',  ( -12.02347592906994223, 46.70319524133616795, -6.153424168697559260 ) ) ;
#556 = APPLICATION_CONTEXT ( 'automotive_design' ) ;
#557 = AXIS2_PLACEMENT_3D ( 'NONE', #4417, #434, #9826 ) ;
#558 = EDGE_CURVE ( 'NONE', #9583, #2472, #6171, .T. ) ;
#559 = CARTESIAN_POINT ( 'NONE',  ( 11.57959441606064210, 45.68864039077092798, -6.943265149869812802 ) ) ;
#560 = CARTESIAN_POINT ( 'NONE',  ( 0.2775435840573023394, 70.17002100411404797, -13.49725908783516992 ) ) ;
#561 = CARTESIAN_POINT ( 'NONE',  ( -3.708203932499369859, 7.663974596215570756, 11.41267819554184193 ) ) ;
#562 = CARTESIAN_POINT ( 'NONE',  ( 5.567119034035452607, 30.97772632656147351, -12.29926522190035598 ) ) ;
#563 = CARTESIAN_POINT ( 'NONE',  ( -13.34493095579965249, 55.85834049113790911, -2.045602713796132122 ) ) ;
#564 = CARTESIAN_POINT ( 'NONE',  ( -2.048896823861042105, 50.60635182041035307, 13.34364247030556250 ) ) ;
#565 = CARTESIAN_POINT ( 'NONE',  ( 7.866633879235673810, 32.97690999812699175, 10.98016867868767577 ) ) ;
#566 = CARTESIAN_POINT ( 'NONE',  ( 10.99999999999990941, 0.000000000000000000, 15.58845726811995824 ) ) ;
#567 = CARTESIAN_POINT ( 'NONE',  ( 12.02160876111696197, 39.65648020511805782, -6.142793857136727986 ) ) ;
#568 = VERTEX_POINT ( 'NONE', #11553 ) ;
#569 = CARTESIAN_POINT ( 'NONE',  ( -8.701713178450388497, 62.34501137507039203, 10.32135525206011728 ) ) ;
#570 = ORIENTED_EDGE ( 'NONE', *, *, #3900, .F. ) ;
#571 = CARTESIAN_POINT ( 'NONE',  ( -13.11924471136216397, 40.81678185826124405, -3.187056428934428087 ) ) ;
#572 = CARTESIAN_POINT ( 'NONE',  ( 13.50000000000000000, 33.43000000000001393, 1.734723475976807094E-15 ) ) ;
#573 = CARTESIAN_POINT ( 'NONE',  ( -18.62500000000064659, -26.01562499999994671, 7.714727599197335195 ) ) ;
#574 = CARTESIAN_POINT ( 'NONE',  ( 13.15187946546656050, 48.32156802418281671, 3.057686379087630968 ) ) ;
#575 = CARTESIAN_POINT ( 'NONE',  ( -10.68872673103600945, 7.854708401161940579, 15.43494339453333808 ) ) ;
#576 = CARTESIAN_POINT ( 'NONE',  ( 13.50000000000000355, 36.57999999999999119, -4.386415899144233244 ) ) ;
#577 = CARTESIAN_POINT ( 'NONE',  ( -0.01842263577481551701, 46.18066228095146641, -13.49998821522327752 ) ) ;
#578 = LINE ( 'NONE', #12865, #13885 ) ;
#579 = CARTESIAN_POINT ( 'NONE',  ( -11.37500000000000178, -67.67499999999981242, -9.545674412382054647E-13 ) ) ;
#580 = CARTESIAN_POINT ( 'NONE',  ( 6.577638901403147109, 53.92217061882819706, 11.78917697844675594 ) ) ;
#581 = EDGE_LOOP ( 'NONE', ( #8546, #6039, #16821, #16086 ) ) ;
#582 = CARTESIAN_POINT ( 'NONE',  ( -8.480464519948240465, 64.50466462916871535, -10.50531813445047113 ) ) ;
#583 = ORIENTED_EDGE ( 'NONE', *, *, #1031, .T. ) ;
#584 = CARTESIAN_POINT ( 'NONE',  ( 3.388210979464494343, 67.05813739842785992, -13.07109493271608436 ) ) ;
#585 = CARTESIAN_POINT ( 'NONE',  ( -5.518765897211704186, 34.38014941849128547, -12.32043976184162837 ) ) ;
#586 = CARTESIAN_POINT ( 'NONE',  ( -8.043339635996302306, -39.54374999999990337, -8.043339635997654113 ) ) ;
#587 = CARTESIAN_POINT ( 'NONE',  ( 4.034064007385466333, 77.82502602479080167, 12.88362052288852055 ) ) ;
#588 = CARTESIAN_POINT ( 'NONE',  ( -16.03410433562986981, 8.027996319639555622, 8.458421099448614200 ) ) ;
#589 = CARTESIAN_POINT ( 'NONE',  ( 0.000000000000000000, 0.000000000000000000, 0.000000000000000000 ) ) ;
#590 = CYLINDRICAL_SURFACE ( 'NONE', #10543, 13.50000000000000000 ) ;
#591 = CARTESIAN_POINT ( 'NONE',  ( 11.10478898303382067, 72.14066452316153288, 7.682293661016322162 ) ) ;
#592 = CARTESIAN_POINT ( 'NONE',  ( 7.272992578804308828, 28.98000000000000398, 10.01041549318726709 ) ) ;
#593 = CARTESIAN_POINT ( 'NONE',  ( -4.171729424061787483, 67.32999999999999829, -12.83926296998457417 ) ) ;
#594 = CARTESIAN_POINT ( 'NONE',  ( -4.026030641589963821, 52.32476109287100741, -12.88609862687250285 ) ) ;
#595 = EDGE_CURVE ( 'NONE', #8209, #16817, #10586, .T. ) ;
#596 = CARTESIAN_POINT ( 'NONE',  ( 7.272992578804311492, 34.87999999999999545, -10.01041549318726709 ) ) ;
#597 = CARTESIAN_POINT ( 'NONE',  ( 13.49999999999999822, 53.27999999999998693, 4.386415899144237684 ) ) ;
#598 = CARTESIAN_POINT ( 'NONE',  ( -8.891200544363830713E-16, 49.67999999999999261, 13.50000000000000000 ) ) ;
#599 = CARTESIAN_POINT ( 'NONE',  ( 9.520470885617715595, -6.869999999999993889, 6.917026985038135400 ) ) ;
#600 = CARTESIAN_POINT ( 'NONE',  ( 9.993611225536259468, 69.07888461794802026, 9.076221008718828642 ) ) ;
#601 = CARTESIAN_POINT ( 'NONE',  ( 12.00000000000003020, 2.713974596215575463, -3.899036354794882531 ) ) ;
#602 = DIRECTION ( 'NONE',  ( -0.000000000000000000, -1.000000000000000000, -0.000000000000000000 ) ) ;
#603 = CARTESIAN_POINT ( 'NONE',  ( 18.62500000000000000, -107.1499999999997783, 1.560692158462880521E-12 ) ) ;
#604 = CARTESIAN_POINT ( 'NONE',  ( -10.51965532506071455, 73.60722549432360040, -8.461029959376727305 ) ) ;
#605 =( BOUNDED_CURVE ( )  B_SPLINE_CURVE ( 2, ( #15515, #15602, #7008, #4844, #16768, #4340, #16347, #4676, #13692, #10167, #14112, #1591, #12384 ),
 .UNSPECIFIED., .F., .F. ) 
 B_SPLINE_CURVE_WITH_KNOTS ( ( 3, 2, 2, 2, 2, 2, 3 ),
 ( 0.5416666666666666297, 0.5444444444444443976, 0.5500000000000000444, 0.5555555555555555802, 0.5611111111111111160, 0.5666666666666666519, 0.5694444444444444198 ),
 .UNSPECIFIED. ) 
 CURVE ( )  GEOMETRIC_REPRESENTATION_ITEM ( )  RATIONAL_B_SPLINE_CURVE ( ( 0.9755282581475768211, 0.9755282581475768211, 1.000000000000000000, 0.9510565162951535312, 1.000000000000000000, 0.9510565162951535312, 1.000000000000000000, 0.9510565162951535312, 1.000000000000000000, 0.9510565162951535312, 1.000000000000000000, 0.9755282581475768211, 0.9755282581475768211 ) ) 
 REPRESENTATION_ITEM ( '' )  );
#606 = CARTESIAN_POINT ( 'NONE',  ( 0.000000000000000000, -8.000000000000000000, 0.000000000000000000 ) ) ;
#607 = DIRECTION ( 'NONE',  ( 0.000000000000000000, -1.000000000000000000, 0.000000000000000000 ) ) ;
#608 = CARTESIAN_POINT ( 'NONE',  ( 20.00000000000000000, 0.000000000000000000, 7.056441485635107799E-14 ) ) ;
#609 = CARTESIAN_POINT ( 'NONE',  ( 10.92172942406179104, 25.73000000000000398, -7.935100905948385908 ) ) ;
#610 = CARTESIAN_POINT ( 'NONE',  ( 11.76794919243112325, -3.569999999999996732, 1.734723475976807094E-15 ) ) ;
#611 = CARTESIAN_POINT ( 'NONE',  ( -11.76794919243112325, 41.92999999999999261, -2.882316262207890869E-15 ) ) ;
#612 = CARTESIAN_POINT ( 'NONE',  ( -11.27205087680846773, 32.20880266355328558, 7.429057979085468943 ) ) ;
#613 = CARTESIAN_POINT ( 'NONE',  ( 2.274101073109970006, 74.76175775842119720, 13.30899290276055069 ) ) ;
#614 = CARTESIAN_POINT ( 'NONE',  ( 1.653273178848926472E-15, 30.93000000000001393, 13.50000000000000000 ) ) ;
#615 = AXIS2_PLACEMENT_3D ( 'NONE', #2922, #15204, #14943 ) ;
#616 = CARTESIAN_POINT ( 'NONE',  ( -8.343458848123582072, 79.37999999999999545, 11.48378591275254124 ) ) ;
#617 = EDGE_CURVE ( 'NONE', #11528, #3781, #9980, .T. ) ;
#618 = CARTESIAN_POINT ( 'NONE',  ( 9.922981821730571639, 51.78482716919520357, -9.154569396628096101 ) ) ;
#619 = DIRECTION ( 'NONE',  ( -0.000000000000000000, 1.000000000000000000, -0.000000000000000000 ) ) ;
#620 = CARTESIAN_POINT ( 'NONE',  ( 1.759800498587698492, 37.11690690510804558, -13.39206196151561912 ) ) ;
#621 = DIRECTION ( 'NONE',  ( 0.000000000000000000, 0.000000000000000000, -1.000000000000000000 ) ) ;
#622 = CARTESIAN_POINT ( 'NONE',  ( 8.549612433556128696E-08, 65.68000242247177312, 13.49999999999999822 ) ) ;
#623 = VECTOR ( 'NONE', #13863, 1000.000000000000000 ) ;
#624 = CARTESIAN_POINT ( 'NONE',  ( 7.135932271715804909, 62.94537907865952064, 11.45987087908721769 ) ) ;
#625 = CARTESIAN_POINT ( 'NONE',  ( 2.967265984436029846, 41.78676304960944066, 13.16990152412644477 ) ) ;
#626 = CARTESIAN_POINT ( 'NONE',  ( 10.00082048966772952, 48.78101140217790288, -9.079552510824187905 ) ) ;
#627 = CARTESIAN_POINT ( 'NONE',  ( 9.520470885617715595, 23.13000000000001322, 6.917026985038135400 ) ) ;
#628 = ORIENTED_EDGE ( 'NONE', *, *, #10569, .F. ) ;
#629 = CARTESIAN_POINT ( 'NONE',  ( -3.636496289402155746, 69.53000000000001535, 11.19198476289190936 ) ) ;
#630 = CARTESIAN_POINT ( 'NONE',  ( 18.62500000000064659, -77.04062499999979252, -7.714727599197336083 ) ) ;
#631 = CARTESIAN_POINT ( 'NONE',  ( 11.37499999999960210, -48.90937499999988347, 4.711679271994917428 ) ) ;
#632 = CARTESIAN_POINT ( 'NONE',  ( -2.081804195782924971, 43.25485282119976205, -13.33860214849647718 ) ) ;
#633 = CARTESIAN_POINT ( 'NONE',  ( -13.35138662365028317, 1.798999282680476490E-09, 1.996909364337476678 ) ) ;
#634 = CARTESIAN_POINT ( 'NONE',  ( 18.62500000000064304, -84.29062499999980673, -7.714727599197334307 ) ) ;
#635 = CARTESIAN_POINT ( 'NONE',  ( 12.91505872096568908, 66.28907917036056574, 3.930856618993244567 ) ) ;
#636 = LINE ( 'NONE', #804, #6795 ) ;
#637 = CARTESIAN_POINT ( 'NONE',  ( 9.520470885617717371, 46.73000000000000398, -6.917026985038131848 ) ) ;
#638 = CARTESIAN_POINT ( 'NONE',  ( 9.235079662642815990, 32.03187319105528985, 10.25657514373247992 ) ) ;
#639 = CARTESIAN_POINT ( 'NONE',  ( -7.272992578804307939, 56.47999999999998977, -10.01041549318726886 ) ) ;
#640 = EDGE_CURVE ( 'NONE', #17255, #13655, #11147, .T. ) ;
#641 = CARTESIAN_POINT ( 'NONE',  ( -10.67851723851311974, 46.61476266519934342, -8.293634792068681705 ) ) ;
#642 = CARTESIAN_POINT ( 'NONE',  ( 5.599984837145694172, 45.97674325351677282, -12.28377481317420816 ) ) ;
#643 = CARTESIAN_POINT ( 'NONE',  ( 7.438616558803111900, 69.90178393563131465, -11.26982506745944512 ) ) ;
#644 = CARTESIAN_POINT ( 'NONE',  ( -21.14483242576211453, 7.170662809914417402, -2.970370385949514080 ) ) ;
#645 = CARTESIAN_POINT ( 'NONE',  ( 10.32066366485157616, 30.76371262851852606, -8.702842429855374817 ) ) ;
#646 = CARTESIAN_POINT ( 'NONE',  ( -11.08589355985044911, 56.22027713396840198, 7.704122408052090698 ) ) ;
#647 = CARTESIAN_POINT ( 'NONE',  ( -2.103279777628626945, 50.60437299590867610, 13.33515391181352605 ) ) ;
#648 = CARTESIAN_POINT ( 'NONE',  ( 2.327276230778790644, 32.76365894630023234, 13.30533770644748159 ) ) ;
#649 = CARTESIAN_POINT ( 'NONE',  ( 3.628474543935842789, 43.04958345259967700, -13.00536312147723095 ) ) ;
#650 = CARTESIAN_POINT ( 'NONE',  ( 12.21724735566978204, 39.64072623559641073, -5.747072418630094326 ) ) ;
#651 = ORIENTED_EDGE ( 'NONE', *, *, #15700, .T. ) ;
#652 = CARTESIAN_POINT ( 'NONE',  ( -13.47981080816064825, 61.90441198062364236, -0.7403440101722559286 ) ) ;
#653 = ORIENTED_EDGE ( 'NONE', *, *, #15929, .T. ) ;
#654 = VECTOR ( 'NONE', #10791, 1000.000000000000000 ) ;
#655 = EDGE_LOOP ( 'NONE', ( #16025, #4531, #10556, #1146 ) ) ;
#656 = CARTESIAN_POINT ( 'NONE',  ( 8.050218389484046000, -18.96812680894470304, 8.940655939244130934 ) ) ;
#657 = CARTESIAN_POINT ( 'NONE',  ( 7.714727599200458030, -36.42187499999990763, -18.62499999999934985 ) ) ;
#658 = CARTESIAN_POINT ( 'NONE',  ( 13.04930443264937523, 48.30669093399095004, 3.459466926551658439 ) ) ;
#659 = CARTESIAN_POINT ( 'NONE',  ( 8.527674399818419460, 57.85321952167059578, -10.46888370426456305 ) ) ;
#660 = CARTESIAN_POINT ( 'NONE',  ( 7.403926216836778984, 78.90321946119443908, -11.28912104649029047 ) ) ;
#661 = CARTESIAN_POINT ( 'NONE',  ( -7.272992578804310604, 81.38000000000000966, 10.01041549318726709 ) ) ;
#662 = CARTESIAN_POINT ( 'NONE',  ( 8.343458848123578520, 37.98000000000000398, 11.48378591275254124 ) ) ;
#663 = CARTESIAN_POINT ( 'NONE',  ( 9.205343071196221416, 2.875466159201993104E-15, -7.970107636079089453 ) ) ;
#664 = CARTESIAN_POINT ( 'NONE',  ( -1.296431213746256139, 7.924856485849755217, 18.46737842244074201 ) ) ;
#665 = DIRECTION ( 'NONE',  ( -0.000000000000000000, 1.000000000000000000, -0.000000000000000000 ) ) ;
#666 = CARTESIAN_POINT ( 'NONE',  ( -8.043339635997654113, -19.80624999999993463, 8.043339635996304082 ) ) ;
#667 = CARTESIAN_POINT ( 'NONE',  ( 3.259877015350815199, 53.79722067765693083, 13.10050803911334327 ) ) ;
#668 = VERTEX_POINT ( 'NONE', #841 ) ;
#669 = LINE ( 'NONE', #8991, #3297 ) ;
#670 = ORIENTED_EDGE ( 'NONE', *, *, #3900, .T. ) ;
#671 = CARTESIAN_POINT ( 'NONE',  ( 2.138189944381238661, 8.756881422320265784, 13.49999999999999822 ) ) ;
#672 = CARTESIAN_POINT ( 'NONE',  ( -5.523541487972947195, 34.38033358995659938, -12.31829916344299214 ) ) ;
#673 = CARTESIAN_POINT ( 'NONE',  ( -8.343458848123576743, 17.48000000000000753, -11.48378591275254301 ) ) ;
#674 = CARTESIAN_POINT ( 'NONE',  ( 11.37500000000000000, -99.89999999999976410, 9.531744055041752924E-13 ) ) ;
#675 = CARTESIAN_POINT ( 'NONE',  ( 4.443323578948271901, 77.83982787778398915, 12.74793837166312827 ) ) ;
#676 = CARTESIAN_POINT ( 'NONE',  ( -17.32050807568884210, 7.773118517290098950, 7.999999999999840128 ) ) ;
#677 = CARTESIAN_POINT ( 'NONE',  ( 15.50029318102139086, 8.062211461649205546, 9.152478727637658906 ) ) ;
#678 = DIRECTION ( 'NONE',  ( 1.224646799147353207E-16, 0.000000000000000000, -1.000000000000000000 ) ) ;
#679 = CARTESIAN_POINT ( 'NONE',  ( 13.37510286910101520, 72.36596172307848462, 1.832109072391795879 ) ) ;
#680 = CARTESIAN_POINT ( 'NONE',  ( 11.76794919243112325, 26.28000000000000824, 3.823638476888996163 ) ) ;
#681 = CARTESIAN_POINT ( 'NONE',  ( 2.607531440858944223E-15, 67.17999999999999261, -14.19474002721660355 ) ) ;
#682 = CARTESIAN_POINT ( 'NONE',  ( -0.09279092634077520940, 71.67666048054469741, 13.49999999999947420 ) ) ;
#683 = CARTESIAN_POINT ( 'NONE',  ( 9.520470885617717371, -15.26999999999999957, -6.917026985038131848 ) ) ;
#684 = CARTESIAN_POINT ( 'NONE',  ( -10.92172942406178926, 57.63000000000000256, -7.935100905948389460 ) ) ;
#685 = CARTESIAN_POINT ( 'NONE',  ( 19.00000000000000711, 7.773118517290098062, -1.732050807568807249 ) ) ;
#686 = CARTESIAN_POINT ( 'NONE',  ( 11.76794919243112325, -0.5699999999999871836, 1.734723475976807094E-15 ) ) ;
#687 = CARTESIAN_POINT ( 'NONE',  ( 2.924053257345435538E-06, 68.68008145904181561, 13.49999999999936584 ) ) ;
#688 = CARTESIAN_POINT ( 'NONE',  ( -13.16986379960055231, -43.70624999999989768, 13.16986379959834252 ) ) ;
#689 = CARTESIAN_POINT ( 'NONE',  ( 15.58845726811984811, 7.773118517290097174, 11.00000000000007283 ) ) ;
#690 = CARTESIAN_POINT ( 'NONE',  ( 18.62500000000064304, -34.34062499999991047, -7.714727599197335195 ) ) ;
#691 = CARTESIAN_POINT ( 'NONE',  ( -13.49546379884621672, 73.91715910944417089, -0.3713218310782592235 ) ) ;
#692 = CARTESIAN_POINT ( 'NONE',  ( -11.51278214438144865, 65.19318789086543120, 7.050241511786378368 ) ) ;
#693 = CARTESIAN_POINT ( 'NONE',  ( 9.708203932499369415, 7.996025403784436492, 7.053423027509680310 ) ) ;
#694 = CARTESIAN_POINT ( 'NONE',  ( 8.000000000000021316, 7.804634910649121515, -17.19094712553552284 ) ) ;
#695 = CARTESIAN_POINT ( 'NONE',  ( -13.49999999999999822, 27.07999999999999474, 4.386415899144235908 ) ) ;
#696 = EDGE_CURVE ( 'NONE', #8605, #6168, #15766, .T. ) ;
#697 = ORIENTED_EDGE ( 'NONE', *, *, #1901, .T. ) ;
#698 = CARTESIAN_POINT ( 'NONE',  ( -3.636496289402155746, 39.52999999999999403, 11.19198476289190936 ) ) ;
#699 = DIRECTION ( 'NONE',  ( 9.637352644315592778E-17, -1.000000000000000000, 0.000000000000000000 ) ) ;
#700 = CARTESIAN_POINT ( 'NONE',  ( 13.50000000000000355, 80.57999999999998408, -4.386415899144233244 ) ) ;
#701 = CARTESIAN_POINT ( 'NONE',  ( -13.47700622531958281, 31.90260597682616961, -0.7909189831980687480 ) ) ;
#702 = CARTESIAN_POINT ( 'NONE',  ( 8.411976504965995360, 75.00153989494273787, 10.55890256502399893 ) ) ;
#703 = CARTESIAN_POINT ( 'NONE',  ( -0.1736909584870764689, 53.67375392313818594, 13.49917744846566947 ) ) ;
#704 = CARTESIAN_POINT ( 'NONE',  ( -13.49999999999999822, 78.78000000000001535, -4.386415899144240349 ) ) ;
#705 = CARTESIAN_POINT ( 'NONE',  ( 12.64183604165299002, 51.60150530966055982, -4.736456310785323254 ) ) ;
#706 =( BOUNDED_CURVE ( )  B_SPLINE_CURVE ( 2, ( #9426, #14775, #11974, #14606, #5437, #2665, #14858, #8096, #31, #10824, #16186, #2488, #1184 ),
 .UNSPECIFIED., .F., .F. ) 
 B_SPLINE_CURVE_WITH_KNOTS ( ( 3, 2, 2, 2, 2, 2, 3 ),
 ( 0.8472222222222222099, 0.8499999999999999778, 0.8555555555555555136, 0.8611111111111111605, 0.8666666666666666963, 0.8722222222222222321, 0.8750000000000000000 ),
 .UNSPECIFIED. ) 
 CURVE ( )  GEOMETRIC_REPRESENTATION_ITEM ( )  RATIONAL_B_SPLINE_CURVE ( ( 0.9755282581475768211, 0.9755282581475768211, 1.000000000000000000, 0.9510565162951535312, 1.000000000000000000, 0.9510565162951535312, 1.000000000000000000, 0.9510565162951535312, 1.000000000000000000, 0.9510565162951535312, 1.000000000000000000, 0.9755282581475768211, 0.9755282581475768211 ) ) 
 REPRESENTATION_ITEM ( '' )  );
#707 = CARTESIAN_POINT ( 'NONE',  ( -10.76081525048536669, 38.23950894326511474, 8.153236926004757024 ) ) ;
#708 = CARTESIAN_POINT ( 'NONE',  ( 10.70183563093194756, 36.74286887062785212, -8.241591107763712287 ) ) ;
#709 = CARTESIAN_POINT ( 'NONE',  ( -4.711679271993001628, -12.45312499999998757, -11.37500000000039613 ) ) ;
#710 = CARTESIAN_POINT ( 'NONE',  ( -10.99999999999979394, 0.000000000000000000, -15.58845726812003996 ) ) ;
#711 = CARTESIAN_POINT ( 'NONE',  ( -0.1280143735402073379, 49.18460186041409088, -13.49947902730419003 ) ) ;
#712 = CARTESIAN_POINT ( 'NONE',  ( 1.753268986668952691E-06, 80.68004880551006863, 13.49999999999977263 ) ) ;
#713 = CARTESIAN_POINT ( 'NONE',  ( 4.918125156431671030, 41.85716231917498931, 12.58089576358123018 ) ) ;
#714 = CARTESIAN_POINT ( 'NONE',  ( 13.49969884940630749, 48.42553229603143450, 0.1310880700171220270 ) ) ;
#715 = CARTESIAN_POINT ( 'NONE',  ( 9.520470885617715595, 11.13000000000000078, 6.917026985038135400 ) ) ;
#716 = FACE_OUTER_BOUND ( 'NONE', #17365, .T. ) ;
#717 = VERTEX_POINT ( 'NONE', #5009 ) ;
#718 = CARTESIAN_POINT ( 'NONE',  ( -11.76794919243112325, 62.78000000000000114, -3.823638476888998827 ) ) ;
#719 = CARTESIAN_POINT ( 'NONE',  ( 8.043339635996302306, -23.96874999999992539, 8.043339635997654113 ) ) ;
#720 = CARTESIAN_POINT ( 'NONE',  ( 4.171729424061789260, 55.83000000000000540, 12.83926296998457417 ) ) ;
#721 = EDGE_CURVE ( 'NONE', #1252, #8781, #12071, .T. ) ;
#722 = CARTESIAN_POINT ( 'NONE',  ( -9.520470885617717371, 31.23000000000000753, 6.917026985038133624 ) ) ;
#723 = CARTESIAN_POINT ( 'NONE',  ( 0.8979998255002190621, 76.14771127606977075, -13.47011368339567028 ) ) ;
#724 = CARTESIAN_POINT ( 'NONE',  ( 9.520470885617715595, 34.13000000000000256, 6.917026985038134512 ) ) ;
#725 = CARTESIAN_POINT ( 'NONE',  ( -18.62499999999935341, -57.23437499999987921, -7.714727599200458918 ) ) ;
#726 = CARTESIAN_POINT ( 'NONE',  ( 10.18058291654429226, 66.08880080020819037, 8.866023803930167091 ) ) ;
#727 = CARTESIAN_POINT ( 'NONE',  ( -8.343458848123576743, 79.48000000000000398, -11.48378591275254301 ) ) ;
#728 = AXIS2_PLACEMENT_3D ( 'NONE', #13183, #2289, #13009 ) ;
#729 = CARTESIAN_POINT ( 'NONE',  ( 3.636496289402157078, 53.03000000000000114, -11.19198476289190936 ) ) ;
#730 = CARTESIAN_POINT ( 'NONE',  ( 10.92172942406179104, 7.730000000000014637, -7.935100905948385908 ) ) ;
#731 = CARTESIAN_POINT ( 'NONE',  ( -12.66924821184278471, 59.09957427317683454, 4.683659793808636174 ) ) ;
#732 = CARTESIAN_POINT ( 'NONE',  ( 13.11471341724209339, 45.54378698212244103, -3.202259077053928760 ) ) ;
#733 = CARTESIAN_POINT ( 'NONE',  ( 10.13354921526377694, 69.77373695534940623, -8.919712814319055383 ) ) ;
#734 = CARTESIAN_POINT ( 'NONE',  ( 1.541208229742722979, 7.854057316169015479, 18.71369360505684298 ) ) ;
#735 = CARTESIAN_POINT ( 'NONE',  ( 13.16708594564997625, 30.53565923579080632, -2.981442588050036147 ) ) ;
#736 = CARTESIAN_POINT ( 'NONE',  ( -13.25266014676319948, 55.83927541273924788, -2.572670256372855402 ) ) ;
#737 = CARTESIAN_POINT ( 'NONE',  ( 0.000000000000000000, 80.93000000000000682, 0.000000000000000000 ) ) ;
#738 = CARTESIAN_POINT ( 'NONE',  ( 9.851210787350034082, 63.78852028479234093, -9.230592214737045609 ) ) ;
#739 = CARTESIAN_POINT ( 'NONE',  ( 5.548650298709674189, 42.97870115387426893, -12.30718966409141402 ) ) ;
#740 = CARTESIAN_POINT ( 'NONE',  ( 10.20108122339417633, 39.77014993735368620, -8.842797910576575049 ) ) ;
#741 = ORIENTED_EDGE ( 'NONE', *, *, #14173, .F. ) ;
#742 = CARTESIAN_POINT ( 'NONE',  ( -9.821826846477060613, 62.29041452375334842, 9.272265874321597323 ) ) ;
#743 = VERTEX_POINT ( 'NONE', #8020 ) ;
#744 = EDGE_CURVE ( 'NONE', #9540, #568, #8793, .T. ) ;
#745 = ORIENTED_EDGE ( 'NONE', *, *, #12188, .T. ) ;
#746 = CARTESIAN_POINT ( 'NONE',  ( -7.272992578804307939, -17.52000000000000313, -10.01041549318726886 ) ) ;
#747 = CARTESIAN_POINT ( 'NONE',  ( 18.62499999999934630, -15.60937499999996270, 7.714727599200467800 ) ) ;
#748 = CARTESIAN_POINT ( 'NONE',  ( 6.741581593082713653, 47.92895949507889242, 11.69643156837649656 ) ) ;
#749 = CARTESIAN_POINT ( 'NONE',  ( 10.51843927637086651, 57.75287643017565387, -8.462433850046046757 ) ) ;
#750 = CARTESIAN_POINT ( 'NONE',  ( 4.994996160112292749, 78.99980127340818115, -12.54197035550941841 ) ) ;
#751 = CARTESIAN_POINT ( 'NONE',  ( 2.272985001014427788E-15, 83.17999999999999261, -12.37355403259654985 ) ) ;
#752 = AXIS2_PLACEMENT_3D ( 'NONE', #7158, #4411, #9822 ) ;
#753 = FILL_AREA_STYLE ('',( #919 ) ) ;
#754 = CARTESIAN_POINT ( 'NONE',  ( 5.441113646577481866, 0.000000000000000000, -25.42428528562854595 ) ) ;
#755 = CARTESIAN_POINT ( 'NONE',  ( -11.37500000000000178, -51.02499999999986358, -9.545674412382054647E-13 ) ) ;
#756 = CARTESIAN_POINT ( 'NONE',  ( 11.45940115419385208, 54.16325699306285912, 7.140252089711898620 ) ) ;
#757 = EDGE_LOOP ( 'NONE', ( #6516, #2368, #5539, #17381, #12216, #2672, #8645, #13726 ) ) ;
#758 = B_SPLINE_CURVE_WITH_KNOTS ( 'NONE', 3,
 ( #15839, #9332, #3744, #9160, #14508, #1088, #6502, #17260, #5172, #15924, #7913, #3833, #11968, #14600, #13288, #1176, #17348, #5259, #2569, #7999, #6667, #12051, #17429, #10728, #16093, #22, #15027, #8086, #7022, #13451, #113, #11079, #11166, #2743, #1516, #16452, #8173, #5781, #1691, #4448, #12133, #9855, #12219, #1606, #6754, #5425, #4087, #9764, #12490, #1426, #9503, #10901, #204, #4355, #289, #6843, #16272, #5610, #15109, #5698, #5519, #1337, #13623, #8263, #2657, #12401, #13706, #10991, #2920, #13537, #6932, #10814, #14940, #8350, #16177, #14850, #3008, #4178, #9590, #2832, #8438, #7106, #12310, #16360, #375, #4267, #9677, #13792, #16541, #7348, #15612, #9199, #11663, #8934, #3607, #7604, #7867, #5032, #14293, #7690, #3520, #11749, #5212, #10602, #4857, #3870, #15966, #10432, #14463, #12899, #12982, #13069, #14637, #865, #2352, #1129, #2524, #2178, #11837, #11921, #10345, #6193, #6541, #954, #15879, #6275, #6366, #15791, #4944, #9285, #15699, #14550, #11580, #9018, #17039, #14375, #16955, #2263, #3698, #10260, #13156, #3786, #9111, #7784, #1042, #17214, #5125, #2435, #13241, #17300, #10947, #9720, #4308, #1558, #13323, #5302, #2788, #1215, #12263, #6626, #5383, #13663, #14719, #9545, #2608, #12005, #8127, #12087, #10684, #16314, #15066, #7952, #17470, #6890, #17387, #16050, #9370, #14983 ),
 .UNSPECIFIED., .F., .F.,
 ( 4, 2, 2, 2, 2, 2, 1, 1, 1, 1, 2, 1, 2, 2, 1, 1, 2, 2, 2, 2, 1, 1, 1, 1, 2, 2, 1, 1, 1, 2, 2, 2, 2, 1, 2, 2, 1, 1, 1, 1, 1, 1, 2, 2, 1, 2, 2, 2, 1, 2, 2, 1, 1, 2, 2, 2, 2, 1, 2, 2, 2, 2, 2, 1, 2, 2, 1, 2, 2, 2, 2, 2, 2, 1, 1, 2, 2, 2, 2, 1, 2, 2, 1, 1, 2, 2, 2, 1, 1, 2, 2, 2, 1, 1, 2, 2, 2, 2, 2, 1, 1, 1, 1, 1, 1, 2, 2, 1, 2, 2, 4 ),
 ( 0.3872708296481242041, 0.3881928204034852392, 0.3891148111588463299, 0.3893453088476865886, 0.3894029332698966672, 0.3894173393754491452, 0.3894317454810016788, 0.3894605576921067458, 0.3895758065365268474, 0.3900368019142073650, 0.3904977972918879381, 0.3906130461363080397, 0.3906418583474131068, 0.3906562644529655848, 0.3906706705585181183, 0.3907282949807281969, 0.3909587926695684557, 0.3918807834249295463, 0.3918951895304820243, 0.3919095956360345578, 0.3919384078471396249, 0.3919960322693496479, 0.3921112811137698051, 0.3923417788026100639, 0.3928027741802905815, 0.3937247649356516721, 0.3941857603133321897, 0.3943010091577523468, 0.3943586335799624254, 0.3943874457910674369, 0.3944162580021724485, 0.3946467556910127072, 0.3955687464463736869, 0.3956263708685837654, 0.3956551830796887770, 0.3956839952907937885, 0.3957992441352139457, 0.3960297418240542044, 0.3964907372017347220, 0.3967212348905749808, 0.3968364837349951380, 0.3968941081572052165, 0.3969085142627576945, 0.3969229203683102281, 0.3969517325794152396, 0.3974127279570957572, 0.3983347187124566813, 0.3992567094678176609, 0.3993719583122378181, 0.3994007705233428296, 0.3994151766288953631, 0.3994295827344478411, 0.3994872071566579197, 0.3997177048454981785, 0.4001787002231786405, 0.4011006909785396202, 0.4015616863562200822, 0.4017921840450603410, 0.4019074328894804427, 0.4019650573116905212, 0.4020226817339005443, 0.4038666632446225035, 0.4043276586223029656, 0.4043852830445130442, 0.4044140952556180557, 0.4044429074667230672, 0.4045581563111432244, 0.4047886539999834277, 0.4057106447553444073, 0.4066326355107053869, 0.4068631331995455902, 0.4069207576217556688, 0.4069351637273082023, 0.4069495698328606803, 0.4069783820439656918, 0.4070936308883857935, 0.4075546262660660890, 0.4080156216437463290, 0.4081308704881664307, 0.4081596826992714422, 0.4081668857520476812, 0.4081740888048239202, 0.4081884949103764537, 0.4082461193325864768, 0.4084766170214266245, 0.4093986077767871601, 0.4095138566212072617, 0.4096291054656273078, 0.4098596031544674556, 0.4103205985321477511, 0.4112425892875082867, 0.4117035846651885822, 0.4118188335096086283, 0.4118764579318186514, 0.4119052701429236629, 0.4119340823540286745, 0.4121645800428688222, 0.4130865707982294133, 0.4132018196426495149, 0.4133170684870696165, 0.4135475661759097088, 0.4140085615535900043, 0.4142390592424301521, 0.4143543080868502537, 0.4144119325090602768, 0.4144263386146128103, 0.4144407447201652883, 0.4144695569312702998, 0.4149305523089505399, 0.4158525430643110199, 0.4167745338196714999 ),
 .UNSPECIFIED. ) ;
#759 = DIRECTION ( 'NONE',  ( -0.000000000000000000, 1.000000000000000000, -0.000000000000000000 ) ) ;
#760 = VERTEX_POINT ( 'NONE', #15288 ) ;
#761 = CARTESIAN_POINT ( 'NONE',  ( 7.444293037381387812, 66.90149083381143669, -11.26317529503627313 ) ) ;
#762 = CARTESIAN_POINT ( 'NONE',  ( 4.711679271993006068, -96.77812499999976126, 11.37500000000039257 ) ) ;
#763 = CARTESIAN_POINT ( 'NONE',  ( 0.000000000000000000, 80.93000000000000682, 0.000000000000000000 ) ) ;
#764 = CARTESIAN_POINT ( 'NONE',  ( -2.148228375852590410, 59.60282902806525840, 13.33692188568706705 ) ) ;
#765 = DIRECTION ( 'NONE',  ( -1.000000000000000000, 0.000000000000000000, -7.483177508809139424E-15 ) ) ;
#766 = CARTESIAN_POINT ( 'NONE',  ( -2.138189944381195584, 5.256881422320269337, -13.50000000000001599 ) ) ;
#767 = CARTESIAN_POINT ( 'NONE',  ( 11.75193945976005239, 72.67664319563640163, -6.644281148718726548 ) ) ;
#768 = CARTESIAN_POINT ( 'NONE',  ( -3.636496289402156190, 31.53000000000000114, 11.19198476289190758 ) ) ;
#769 = CARTESIAN_POINT ( 'NONE',  ( 4.171729424061791924, 49.02999999999999403, -12.83926296998457239 ) ) ;
#770 = CARTESIAN_POINT ( 'NONE',  ( -0.3780938980182780851, 71.66640514842048049, 13.49470503427916945 ) ) ;
#771 = CARTESIAN_POINT ( 'NONE',  ( -8.691771469529815392E-16, 52.67999999999999261, 14.19474002721660355 ) ) ;
#772 = CARTESIAN_POINT ( 'NONE',  ( 2.138189944381248875, 76.75688142232026223, 13.49999999999999645 ) ) ;
#773 = EDGE_CURVE ( 'NONE', #2050, #13044, #10025, .T. ) ;
#774 = CARTESIAN_POINT ( 'NONE',  ( 1.966889197916937837, 68.75072210823383045, 13.35595523036250576 ) ) ;
#775 = CARTESIAN_POINT ( 'NONE',  ( -7.714727599197335195, -55.15312499999986784, -18.62500000000064304 ) ) ;
#776 = CARTESIAN_POINT ( 'NONE',  ( 7.329991333342587012, -1.736202706843530252E-17, -9.501117147637041072 ) ) ;
#777 = CARTESIAN_POINT ( 'NONE',  ( 7.714727599197338748, -30.17812499999993747, 18.62500000000063949 ) ) ;
#778 = CARTESIAN_POINT ( 'NONE',  ( -5.177089779691129046, 65.49289956726600792, 12.46787024327672633 ) ) ;
#779 = CARTESIAN_POINT ( 'NONE',  ( 13.14483242576216782, 7.170662809914417402, -16.82677684650029093 ) ) ;
#780 = DIRECTION ( 'NONE',  ( -0.000000000000000000, 1.000000000000000000, -0.000000000000000000 ) ) ;
#781 = ORIENTED_EDGE ( 'NONE', *, *, #5478, .F. ) ;
#782 = CARTESIAN_POINT ( 'NONE',  ( -9.520470885617715595, 32.63000000000000256, -6.917026985038136289 ) ) ;
#783 = CARTESIAN_POINT ( 'NONE',  ( -3.042841478767011054, 40.28940726252261584, -13.15311736850856938 ) ) ;
#784 = CARTESIAN_POINT ( 'NONE',  ( -12.03159204543364780, 32.15617227854212246, 6.137766210929217259 ) ) ;
#785 = CARTESIAN_POINT ( 'NONE',  ( 3.375819219972439278, 74.80137919260076274, 13.07174965501556230 ) ) ;
#786 = LINE ( 'NONE', #15444, #1757 ) ;
#787 = CARTESIAN_POINT ( 'NONE',  ( 13.46198083254162725, 51.46580788858824462, -1.034634726011374184 ) ) ;
#788 = CARTESIAN_POINT ( 'NONE',  ( -11.18084545031510402, 38.21448949798586625, 7.565677266412778046 ) ) ;
#789 = CARTESIAN_POINT ( 'NONE',  ( 12.44984635716159715, 36.62057801016818104, -5.234570041864336609 ) ) ;
#790 = CARTESIAN_POINT ( 'NONE',  ( -8.043339635997652337, -34.30624999999993463, 8.043339635996300530 ) ) ;
#791 = DIRECTION ( 'NONE',  ( 1.000000000000000000, 0.000000000000000000, 3.741588754404567345E-15 ) ) ;
#792 = CARTESIAN_POINT ( 'NONE',  ( -7.030094859684152375, 77.41919333245768087, 11.52885090067665175 ) ) ;
#793 = CARTESIAN_POINT ( 'NONE',  ( -7.999999999999776179, 0.000000000000000000, -17.32050807568887762 ) ) ;
#794 = CARTESIAN_POINT ( 'NONE',  ( 0.2843415538626123951, 41.69023294723046291, 13.49779373366518698 ) ) ;
#795 = CARTESIAN_POINT ( 'NONE',  ( 12.23498167705813344, 48.63917152218695605, -5.705760255632154276 ) ) ;
#796 = CARTESIAN_POINT ( 'NONE',  ( -3.636496289402152637, 15.33000000000001073, -11.19198476289190936 ) ) ;
#797 = EDGE_LOOP ( 'NONE', ( #2942, #3741, #4895, #12420 ) ) ;
#798 = CARTESIAN_POINT ( 'NONE',  ( 9.520470885617715595, 70.12999999999999545, 6.917026985038134512 ) ) ;
#799 = CARTESIAN_POINT ( 'NONE',  ( 9.538709233711902776E-13, 3.087500000000011458, -11.37500000000000178 ) ) ;
#800 = CARTESIAN_POINT ( 'NONE',  ( -9.552639591052204498E-13, -95.73749999999976978, 11.37500000000000000 ) ) ;
#801 = CARTESIAN_POINT ( 'NONE',  ( -7.409984580736203970E-16, 31.68000000000000682, 12.37355403259654985 ) ) ;
#802 = CARTESIAN_POINT ( 'NONE',  ( -11.52888015854885317, 80.93000000000003524, -3.329402692648984363 ) ) ;
#803 = CARTESIAN_POINT ( 'NONE',  ( 18.62499999999934985, -82.20937499999980957, 7.714727599200467800 ) ) ;
#804 = CARTESIAN_POINT ( 'NONE',  ( -24.73863375370587292, 0.000000000000000000, -8.000000000000280664 ) ) ;
#805 =( BOUNDED_CURVE ( )  B_SPLINE_CURVE ( 2, ( #9577, #16439, #10803, #7009, #13693, #13777, #8514, #4341, #15187, #362, #5767, #5414, #1592 ),
 .UNSPECIFIED., .F., .F. ) 
 B_SPLINE_CURVE_WITH_KNOTS ( ( 3, 2, 2, 2, 2, 2, 3 ),
 ( 0.2049045012548912914, 0.2086589264430994406, 0.2161677768195154337, 0.2236766271959315655, 0.2311854775723475863, 0.2386943279487635516, 0.2424487531369445559 ),
 .UNSPECIFIED. ) 
 CURVE ( )  GEOMETRIC_REPRESENTATION_ITEM ( )  RATIONAL_B_SPLINE_CURVE ( ( 0.9755282581475768211, 0.9755282581475758219, 1.000000000000000000, 0.9510565162951536422, 1.000000000000000000, 0.9510565162951536422, 1.000000000000000000, 0.9510565162951536422, 1.000000000000000000, 0.9510565162951536422, 1.000000000000000000, 0.9755282581477529025, 0.9755282581475768211 ) ) 
 REPRESENTATION_ITEM ( '' )  );
#806 = CARTESIAN_POINT ( 'NONE',  ( 3.636496289402157078, 50.03000000000000114, -11.19198476289190936 ) ) ;
#807 = CARTESIAN_POINT ( 'NONE',  ( -13.48016638762386599, 58.90472283406352716, -0.7316414589621201836 ) ) ;
#808 = CARTESIAN_POINT ( 'NONE',  ( 13.50576839576328148, 45.45902382363403404, -0.8387148265821507964 ) ) ;
#809 = CARTESIAN_POINT ( 'NONE',  ( 5.653963835669364002, 69.97463459799799068, -12.25898929304140950 ) ) ;
#810 = ADVANCED_FACE ( 'NONE', ( #7365 ), #1474, .F. ) ;
#811 = FACE_OUTER_BOUND ( 'NONE', #15308, .T. ) ;
#812 = CARTESIAN_POINT ( 'NONE',  ( 13.32379934013461309, 30.35364490307813057, 2.175025330243249400 ) ) ;
#813 = CARTESIAN_POINT ( 'NONE',  ( -13.47793799092467637, 55.90337191138781492, -0.7714925420567289027 ) ) ;
#814 = CARTESIAN_POINT ( 'NONE',  ( -12.91175531483703054, 50.07169591931079822, 3.951675568982145226 ) ) ;
#815 = CARTESIAN_POINT ( 'NONE',  ( 1.109962791137624416, 64.14012643174706341, -13.46178866848010536 ) ) ;
#816 = LINE ( 'NONE', #900, #2037 ) ;
#817 = CARTESIAN_POINT ( 'NONE',  ( 13.07068574514433656, 39.55030779099601546, -3.378615318188594951 ) ) ;
#818 = ORIENTED_EDGE ( 'NONE', *, *, #16024, .T. ) ;
#819 = CARTESIAN_POINT ( 'NONE',  ( -11.98598919180274436, 61.70066361133849853, -6.212500231099927106 ) ) ;
#820 = ORIENTED_EDGE ( 'NONE', *, *, #10454, .T. ) ;
#821 = ORIENTED_EDGE ( 'NONE', *, *, #14507, .F. ) ;
#822 = CARTESIAN_POINT ( 'NONE',  ( -4.171729424061787483, 28.32999999999999474, -12.83926296998457417 ) ) ;
#823 = CARTESIAN_POINT ( 'NONE',  ( -7.714727599197335195, -38.50312499999991189, -18.62500000000064304 ) ) ;
#824 = CARTESIAN_POINT ( 'NONE',  ( 11.54494251065839450, 57.69100095235108938, -6.997463023747798161 ) ) ;
#825 = CARTESIAN_POINT ( 'NONE',  ( 5.294469476691438636, 78.98865934249140253, -12.42107284422839975 ) ) ;
#826 = VECTOR ( 'NONE', #344, 1000.000000000000000 ) ;
#827 = CARTESIAN_POINT ( 'NONE',  ( -11.76794919243112325, 80.93000000000000682, -2.882316262207890869E-15 ) ) ;
#828 = CARTESIAN_POINT ( 'NONE',  ( -13.50000000000000000, 39.92999999999999972, -3.306546357697853733E-15 ) ) ;
#829 = CARTESIAN_POINT ( 'NONE',  ( 0.07528598782886079810, 65.68270963596916090, 13.50000000000771827 ) ) ;
#830 = CARTESIAN_POINT ( 'NONE',  ( 2.222800136090958073E-15, 3.046025403784441643, -12.00000000000000000 ) ) ;
#831 = SURFACE_SIDE_STYLE ('',( #14256 ) ) ;
#832 = CARTESIAN_POINT ( 'NONE',  ( -7.499999999999996447, -18.00000000000000355, 8.999999999999998224 ) ) ;
#833 = CARTESIAN_POINT ( 'NONE',  ( 8.043339635997652337, -44.78124999999987921, -8.043339635996304082 ) ) ;
#834 = CARTESIAN_POINT ( 'NONE',  ( -8.343458848123578520, 78.47999999999998977, -11.48378591275254124 ) ) ;
#835 = CARTESIAN_POINT ( 'NONE',  ( 3.981673202811145451, 34.03692019505243138, -12.90035025641783584 ) ) ;
#836 = ORIENTED_EDGE ( 'NONE', *, *, #12423, .T. ) ;
#837 = CARTESIAN_POINT ( 'NONE',  ( 7.347880794884122694E-16, 0.000000000000000000, -18.00000000000000000 ) ) ;
#838 = EDGE_LOOP ( 'NONE', ( #11462, #9974, #13042, #2651 ) ) ;
#839 = CARTESIAN_POINT ( 'NONE',  ( 16.64104048077464171, 7.924936010579561874, -8.111079018422952203 ) ) ;
#840 = CARTESIAN_POINT ( 'NONE',  ( 8.043339635996300530, -81.16874999999980389, 8.043339635997654113 ) ) ;
#841 = CARTESIAN_POINT ( 'NONE',  ( 2.445080149700053643E-15, 42.17999999999999261, -13.50000000000000000 ) ) ;
#842 = CARTESIAN_POINT ( 'NONE',  ( -0.08603315895956636927, 59.67690236815970195, 13.49999999999913136 ) ) ;
#843 = CARTESIAN_POINT ( 'NONE',  ( 12.00000000000000533, 98.93000000000002103, 1.224646799147353059E-15 ) ) ;
#844 = CARTESIAN_POINT ( 'NONE',  ( 12.50000000000000000, 98.93000000000002103, 1.224646799147353059E-15 ) ) ;
#845 = CARTESIAN_POINT ( 'NONE',  ( 1.326799508617756862, 71.72767848700497950, 13.44100117757941071 ) ) ;
#846 = CARTESIAN_POINT ( 'NONE',  ( 8.343458848123583849, 54.87999999999999545, -11.48378591275253768 ) ) ;
#847 = CARTESIAN_POINT ( 'NONE',  ( -5.550346829431017426, 52.38132149445374353, -12.30848393326122903 ) ) ;
#848 = EDGE_CURVE ( 'NONE', #6168, #7996, #5214, .T. ) ;
#849 = DIRECTION ( 'NONE',  ( 0.000000000000000000, 0.000000000000000000, 1.000000000000000000 ) ) ;
#850 = CARTESIAN_POINT ( 'NONE',  ( 13.16986379959834075, -64.51874999999984084, 13.16986379960055231 ) ) ;
#851 = CARTESIAN_POINT ( 'NONE',  ( 2.310673249324077805, 68.76308373099037397, 13.30456027256653506 ) ) ;
#852 = CARTESIAN_POINT ( 'NONE',  ( -7.714727599200467800, -28.09687499999992966, 18.62499999999934630 ) ) ;
#853 = CARTESIAN_POINT ( 'NONE',  ( 8.244216993401655813, 54.86656887803838600, -10.69961692430309519 ) ) ;
#854 = CARTESIAN_POINT ( 'NONE',  ( 18.62499999999934630, -32.25937499999992042, 7.714727599200467800 ) ) ;
#855 = CARTESIAN_POINT ( 'NONE',  ( -5.222546564494585652, 65.49121520183372525, 12.44892348364579959 ) ) ;
#856 = FACE_OUTER_BOUND ( 'NONE', #7014, .T. ) ;
#857 = CARTESIAN_POINT ( 'NONE',  ( -11.89990621330880316, 40.69421425333050735, -6.375126892817447377 ) ) ;
#858 = CARTESIAN_POINT ( 'NONE',  ( -4.245309975859792750, 35.52737123023494803, 12.81530032056034685 ) ) ;
#859 = CARTESIAN_POINT ( 'NONE',  ( -8.343458848123576743, 23.48000000000000398, -11.48378591275254301 ) ) ;
#860 = VERTEX_POINT ( 'NONE', #5757 ) ;
#861 = DIRECTION ( 'NONE',  ( 0.000000000000000000, 0.000000000000000000, -1.000000000000000000 ) ) ;
#862 = FACE_OUTER_BOUND ( 'NONE', #9261, .T. ) ;
#863 = CARTESIAN_POINT ( 'NONE',  ( -11.84847161218580958, 31.69039032213071749, -6.470251712010556489 ) ) ;
#864 = DIRECTION ( 'NONE',  ( 0.000000000000000000, -0.000000000000000000, 1.000000000000000000 ) ) ;
#865 = CARTESIAN_POINT ( 'NONE',  ( 11.66667137561951506, 60.17734808128163593, 6.792565863938680337 ) ) ;
#866 = CARTESIAN_POINT ( 'NONE',  ( -13.50000000000000000, -0.06999999999998673950, -3.469446951953614189E-15 ) ) ;
#867 = CARTESIAN_POINT ( 'NONE',  ( 0.000000000000000000, 80.93000000000000682, 0.000000000000000000 ) ) ;
#868 =( NAMED_UNIT ( * ) SI_UNIT ( $, .STERADIAN. ) SOLID_ANGLE_UNIT ( ) );
#869 = CARTESIAN_POINT ( 'NONE',  ( -8.691771469529815392E-16, 73.67999999999999261, 14.19474002721660355 ) ) ;
#870 = CARTESIAN_POINT ( 'NONE',  ( 11.70511894169415790, 51.67995204303867496, -6.726098610477120765 ) ) ;
#871 = CARTESIAN_POINT ( 'NONE',  ( -13.33075286816964322, 38.00475805412492036, 2.131075495770263117 ) ) ;
#872 = CARTESIAN_POINT ( 'NONE',  ( 13.07195708592954730, 36.55011500055716311, -3.373404994585333938 ) ) ;
#873 = CARTESIAN_POINT ( 'NONE',  ( 11.37499999999999645, -40.54999999999992610, 9.531744055041752924E-13 ) ) ;
#874 = CARTESIAN_POINT ( 'NONE',  ( 3.708203932499368527, 1.696025403784435781, 11.41267819554184371 ) ) ;
#875 = CARTESIAN_POINT ( 'NONE',  ( -11.06054324169216230, 77.22177975307495501, 7.745344326915604150 ) ) ;
#876 = CARTESIAN_POINT ( 'NONE',  ( -4.416226258374795322, 80.52113410087463308, 12.75764956076284840 ) ) ;
#877 = CARTESIAN_POINT ( 'NONE',  ( 0.1409280224492138189, 41.68508833901529442, 13.49999999997910116 ) ) ;
#878 = ORIENTED_EDGE ( 'NONE', *, *, #4542, .T. ) ;
#879 = CARTESIAN_POINT ( 'NONE',  ( 11.76794919243112325, 14.28000000000000647, 3.823638476888996163 ) ) ;
#880 = DIRECTION ( 'NONE',  ( 0.000000000000000000, -1.000000000000000000, 0.000000000000000000 ) ) ;
#881 = ORIENTED_EDGE ( 'NONE', *, *, #14946, .T. ) ;
#882 = CARTESIAN_POINT ( 'NONE',  ( -3.636496289402155746, 57.53000000000000114, 11.19198476289190936 ) ) ;
#883 = CARTESIAN_POINT ( 'NONE',  ( -4.711679271993003404, -47.90312499999986784, -11.37500000000039613 ) ) ;
#884 = CARTESIAN_POINT ( 'NONE',  ( -17.32050807568865736, 0.000000000000000000, -10.00000000000020428 ) ) ;
#885 = CARTESIAN_POINT ( 'NONE',  ( -8.343458848123582072, -0.6200000000000037703, 11.48378591275254124 ) ) ;
#886 = CARTESIAN_POINT ( 'NONE',  ( 0.8688120066860616220, 76.14876072707028243, -13.47201481489776675 ) ) ;
#887 = CARTESIAN_POINT ( 'NONE',  ( -18.62499999999935341, -90.53437499999978400, -7.714727599200458918 ) ) ;
#888 = CARTESIAN_POINT ( 'NONE',  ( 0.000000000000000000, 9.000000000000000000, 0.000000000000000000 ) ) ;
#889 = CARTESIAN_POINT ( 'NONE',  ( -11.76794919243112325, 51.07999999999999829, 3.823638476888994386 ) ) ;
#890 = LINE ( 'NONE', #1157, #7795 ) ;
#891 = CARTESIAN_POINT ( 'NONE',  ( -12.14234156378920737, 59.14700413339190277, 5.904461971908546047 ) ) ;
#892 = CARTESIAN_POINT ( 'NONE',  ( 10.42207727469415524, 45.10182129088688185, 8.580813032019420916 ) ) ;
#893 = CARTESIAN_POINT ( 'NONE',  ( 13.40814881853847318, 69.37525059538582184, 1.572674541139606141 ) ) ;
#894 = CIRCLE ( 'NONE', #12755, 12.00000000000000178 ) ;
#895 = CARTESIAN_POINT ( 'NONE',  ( 4.274400199475617335, 80.83369808617747765, 12.80560251886253731 ) ) ;
#896 = CARTESIAN_POINT ( 'NONE',  ( 11.95805636813460104, 30.66140720589453039, -6.265947899127372267 ) ) ;
#897 = CARTESIAN_POINT ( 'NONE',  ( -12.51544737404857344, 56.11421971867084579, 5.067590151480188432 ) ) ;
#898 = CARTESIAN_POINT ( 'NONE',  ( -5.838308194493356140, 50.46740077971483629, 12.17325453446762040 ) ) ;
#899 = CARTESIAN_POINT ( 'NONE',  ( 5.325587175574985288, 63.98723509382200803, -12.40517262089496597 ) ) ;
#900 = CARTESIAN_POINT ( 'NONE',  ( 1.653273178848926472E-15, 80.93000000000000682, 13.50000000000000000 ) ) ;
#901 = CARTESIAN_POINT ( 'NONE',  ( 11.98396937526130124, 39.65939841873632332, -6.215724125712108972 ) ) ;
#902 = VERTEX_POINT ( 'NONE', #13766 ) ;
#903 = LINE ( 'NONE', #11788, #7523 ) ;
#904 = CARTESIAN_POINT ( 'NONE',  ( -10.05880256514230986, 61.58230886132751891, -9.003917470233888665 ) ) ;
#905 = CARTESIAN_POINT ( 'NONE',  ( 11.76794919243112325, 5.430000000000004157, 1.734723475976807094E-15 ) ) ;
#906 = ORIENTED_EDGE ( 'NONE', *, *, #10979, .F. ) ;
#907 = CARTESIAN_POINT ( 'NONE',  ( -10.43129681812944476, 40.60213892834825344, -8.569776200266453259 ) ) ;
#908 = VERTEX_POINT ( 'NONE', #12466 ) ;
#909 = CARTESIAN_POINT ( 'NONE',  ( -10.92172942406178926, 31.63000000000002032, -7.935100905948389460 ) ) ;
#910 = CARTESIAN_POINT ( 'NONE',  ( -1.564113515457998370E-12, -86.33749999999982094, 18.62500000000000000 ) ) ;
#911 = EDGE_CURVE ( 'NONE', #7559, #9213, #3287, .T. ) ;
#912 = CARTESIAN_POINT ( 'NONE',  ( 5.012090283648058531, 47.86087352477124313, 12.53511619697896329 ) ) ;
#913 = AXIS2_PLACEMENT_3D ( 'NONE', #4187, #4365, #9687 ) ;
#914 = CARTESIAN_POINT ( 'NONE',  ( 11.55553819978283769, 57.69029574722926412, -6.979941511154718725 ) ) ;
#915 = CARTESIAN_POINT ( 'NONE',  ( 7.183560718835745540, 78.91260539477536895, -11.43007281236147143 ) ) ;
#916 = CARTESIAN_POINT ( 'NONE',  ( 3.636496289402157078, 83.03000000000000114, -11.19198476289190936 ) ) ;
#917 = CARTESIAN_POINT ( 'NONE',  ( 8.120631507080247502, 3.937340487231679721E-15, -8.939559169390870252 ) ) ;
#918 = CARTESIAN_POINT ( 'NONE',  ( 12.50000000000000000, -18.00000000000000355, -2.204364238465235822E-15 ) ) ;
#919 = FILL_AREA_STYLE_COLOUR ( '', #3062 ) ;
#920 = DIRECTION ( 'NONE',  ( 0.000000000000000000, 1.000000000000000000, 0.000000000000000000 ) ) ;
#921 = CARTESIAN_POINT ( 'NONE',  ( 8.043339635997652337, -61.43124999999983515, -8.043339635996304082 ) ) ;
#922 = CIRCLE ( 'NONE', #10257, 4.000000000000004441 ) ;
#923 = LINE ( 'NONE', #5273, #11771 ) ;
#924 = CARTESIAN_POINT ( 'NONE',  ( 3.020329884759706207, 34.07140041091936666, -13.15781035347679229 ) ) ;
#925 = ORIENTED_EDGE ( 'NONE', *, *, #16490, .T. ) ;
#926 = CARTESIAN_POINT ( 'NONE',  ( 8.464728390624178894E-06, 46.17999963826949994, -13.49999999999734790 ) ) ;
#927 = ORIENTED_EDGE ( 'NONE', *, *, #8049, .F. ) ;
#928 = CARTESIAN_POINT ( 'NONE',  ( -10.92172942406178926, 16.63000000000000611, -7.935100905948389460 ) ) ;
#929 = CARTESIAN_POINT ( 'NONE',  ( -8.043339635996300530, -30.14374999999994742, -8.043339635997652337 ) ) ;
#930 = CARTESIAN_POINT ( 'NONE',  ( 25.42428528562856727, 0.000000000000000000, -5.441113646577394825 ) ) ;
#931 = CARTESIAN_POINT ( 'NONE',  ( -4.454599061965374140, 59.51975211702684021, 12.75138711840418893 ) ) ;
#932 = CARTESIAN_POINT ( 'NONE',  ( 8.000000000000023093, 0.000000000000000000, -17.32050807568876394 ) ) ;
#933 = EDGE_CURVE ( 'NONE', #11898, #2603, #4937, .T. ) ;
#934 = CARTESIAN_POINT ( 'NONE',  ( -2.138187238715951288, 6.603118674965478441, 13.50000087912394520 ) ) ;
#935 = CARTESIAN_POINT ( 'NONE',  ( -4.171729424061791036, 53.52999999999999403, 12.83926296998457239 ) ) ;
#936 = CARTESIAN_POINT ( 'NONE',  ( -5.052807978041880865, 71.49763661691018513, 12.52071977299732630 ) ) ;
#937 = CARTESIAN_POINT ( 'NONE',  ( 13.49999999999999822, 77.27999999999998693, 4.386415899144236796 ) ) ;
#938 = CARTESIAN_POINT ( 'NONE',  ( -13.16986379959834252, -56.19374999999985931, -13.16986379960055054 ) ) ;
#939 = CARTESIAN_POINT ( 'NONE',  ( 1.977490458657884753, 68.75110324043748733, 13.35439718596144765 ) ) ;
#940 = CARTESIAN_POINT ( 'NONE',  ( -7.714727599200467800, -44.74687499999989626, 18.62499999999934630 ) ) ;
#941 = DIRECTION ( 'NONE',  ( 0.000000000000000000, 1.000000000000000000, 0.000000000000000000 ) ) ;
#942 = CARTESIAN_POINT ( 'NONE',  ( 18.62500000000000000, -66.59999999999983800, 1.560692158462880521E-12 ) ) ;
#943 = CARTESIAN_POINT ( 'NONE',  ( -5.384056574969746656, 65.48512799171378163, 12.38010029700703996 ) ) ;
#944 = CARTESIAN_POINT ( 'NONE',  ( 2.894739436579920166E-06, 50.68008041434205069, 13.49999999999938005 ) ) ;
#945 = CARTESIAN_POINT ( 'NONE',  ( -11.25500439539402464, 35.20987436177090046, 7.454859297479469404 ) ) ;
#946 = CARTESIAN_POINT ( 'NONE',  ( -4.171729424061787483, 23.33000000000001606, -12.83926296998457417 ) ) ;
#947 = ORIENTED_EDGE ( 'NONE', *, *, #7215, .F. ) ;
#948 = CARTESIAN_POINT ( 'NONE',  ( 2.138189944381242213, 51.10311857767973009, -13.49999999999999822 ) ) ;
#949 = CYLINDRICAL_SURFACE ( 'NONE', #11715, 12.00000000000000178 ) ;
#950 = CARTESIAN_POINT ( 'NONE',  ( 11.37500000000000000, -9.629649721936179265E-32, 9.531744055041752924E-13 ) ) ;
#951 = ADVANCED_FACE ( 'NONE', ( #862 ), #949, .F. ) ;
#952 = CARTESIAN_POINT ( 'NONE',  ( -12.49172365619227598, 32.11631608597728871, 5.120886946257767747 ) ) ;
#953 = FACE_OUTER_BOUND ( 'NONE', #2430, .T. ) ;
#954 = CARTESIAN_POINT ( 'NONE',  ( 11.24200432374102299, 60.14937899929235243, 7.477721340839896591 ) ) ;
#955 = CARTESIAN_POINT ( 'NONE',  ( 13.50000000000000000, -10.56999999999999673, 1.734723475976807094E-15 ) ) ;
#956 = CARTESIAN_POINT ( 'NONE',  ( -7.158319469831337045, 53.41367405225197018, 11.44589433405317536 ) ) ;
#957 = CARTESIAN_POINT ( 'NONE',  ( -11.76794919243112325, 59.92999999999999972, -2.882316262207890869E-15 ) ) ;
#958 = CARTESIAN_POINT ( 'NONE',  ( 13.50000000000000000, 77.42999999999999261, 1.653273178848926867E-15 ) ) ;
#959 = CARTESIAN_POINT ( 'NONE',  ( 13.49112894113379646, 51.44683640026539706, -0.4894624279518585142 ) ) ;
#960 = CARTESIAN_POINT ( 'NONE',  ( -9.629163158805681633, 38.29992217420160472, 9.465125892876324443 ) ) ;
#961 = CARTESIAN_POINT ( 'NONE',  ( 11.23715272735747206, 36.71099532258286047, -7.481738776993401174 ) ) ;
#962 = CARTESIAN_POINT ( 'NONE',  ( 11.37499999999960210, -56.15937499999989058, 4.711679271994916540 ) ) ;
#963 = CARTESIAN_POINT ( 'NONE',  ( -5.417673612917023540, 74.48380672519944312, 12.36591168787385087 ) ) ;
#964 = CARTESIAN_POINT ( 'NONE',  ( 1.982521523170245906E-06, 77.68005525700222336, 13.49999999999970690 ) ) ;
#965 = CARTESIAN_POINT ( 'NONE',  ( -4.708371381723156723, 80.51042602726658970, 12.65400907433436117 ) ) ;
#966 = CYLINDRICAL_SURFACE ( 'NONE', #9419, 13.50000000000000000 ) ;
#967 = VERTEX_POINT ( 'NONE', #7344 ) ;
#968 = CARTESIAN_POINT ( 'NONE',  ( -7.409984580736203970E-16, 13.67999999999999616, 12.37355403259654985 ) ) ;
#969 = DIRECTION ( 'NONE',  ( -0.000000000000000000, -1.000000000000000000, -0.000000000000000000 ) ) ;
#970 = ORIENTED_EDGE ( 'NONE', *, *, #15747, .T. ) ;
#971 = CARTESIAN_POINT ( 'NONE',  ( 9.520470885617717371, 55.73000000000000398, -6.917026985038131848 ) ) ;
#972 = CARTESIAN_POINT ( 'NONE',  ( -4.711679271994916540, -37.49687499999989626, 11.37499999999960565 ) ) ;
#973 = CARTESIAN_POINT ( 'NONE',  ( -11.37500000000000000, -91.57499999999977547, -9.545674412382054647E-13 ) ) ;
#974 = B_SPLINE_CURVE_WITH_KNOTS ( 'NONE', 3,
 ( #15714, #3972, #5048, #13169, #2623, #8056, #11852, #3618, #9034, #13337, #13420, #1309, #9127, #17227, #2364, #7967, #14735, #2277, #14388, #7704, #7798, #7878, #9384, #17314, #5228, #10445, #9212, #15980, #1055, #6467, #10699, #6724, #12102, #13256, #1143, #4957, #15892, #3883, #5138, #6554, #16066, #14651, #6640, #10613 ),
 .UNSPECIFIED., .F., .F.,
 ( 4, 2, 2, 2, 2, 2, 2, 2, 2, 2, 2, 2, 2, 2, 2, 2, 2, 2, 2, 2, 2, 4 ),
 ( 0.03689401835950767428, 0.03766257893388839234, 0.03843113950826911041, 0.03919970008264982847, 0.03996826065703055347, 0.04073682123141127154, 0.04150538180579198960, 0.04304250295455346043, 0.04457962410331492431, 0.04611674525207638820, 0.04765386640083785902, 0.04919098754959932984, 0.05072810869836079373, 0.05226522984712225761, 0.05380235099588372844, 0.05533947214464519232, 0.05687659329340666314, 0.05764515386778737427, 0.05841371444216809927, 0.05995083559092950765, 0.06071939616531019102, 0.06148795673969087439 ),
 .UNSPECIFIED. ) ;
#975 = CARTESIAN_POINT ( 'NONE',  ( 12.17141580355952080, 75.64447568897026031, -5.840979099278275299 ) ) ;
#976 = CARTESIAN_POINT ( 'NONE',  ( -1.010931998681471075E-07, 71.67999718330101189, 13.49999999999999822 ) ) ;
#977 = VECTOR ( 'NONE', #10428, 999.9999999999998863 ) ;
#978 = CARTESIAN_POINT ( 'NONE',  ( -13.50000000000000000, 73.92999999999999261, -3.306546357697853733E-15 ) ) ;
#979 = CARTESIAN_POINT ( 'NONE',  ( -11.76794919243112325, 47.77999999999999403, -3.823638476888998827 ) ) ;
#980 = CARTESIAN_POINT ( 'NONE',  ( -3.708203932499385846, 9.463974596215601665, -11.41267819554190233 ) ) ;
#981 = CARTESIAN_POINT ( 'NONE',  ( -11.07966164616091298, 59.22065182733356181, 7.713049733970735566 ) ) ;
#982 = CARTESIAN_POINT ( 'NONE',  ( 13.40951939699013806, 45.37387384954418224, 1.609924743746272036 ) ) ;
#983 = CARTESIAN_POINT ( 'NONE',  ( 10.56082941162724609, 69.75074268295333013, -8.413808112793510929 ) ) ;
#984 = CARTESIAN_POINT ( 'NONE',  ( 0.2979893671971325930, 80.69079410851497869, 13.49999999993527311 ) ) ;
#985 = CARTESIAN_POINT ( 'NONE',  ( 13.49835112770431955, 30.43830851857264008, -0.2430632257887174463 ) ) ;
#986 = EDGE_CURVE ( 'NONE', #11811, #7222, #9746, .T. ) ;
#987 = CARTESIAN_POINT ( 'NONE',  ( -4.651663545995293525, 55.34748731497323604, -12.67467349376107677 ) ) ;
#988 = CARTESIAN_POINT ( 'NONE',  ( -12.66557966946106184, 50.09907455509510044, 4.673096744009077597 ) ) ;
#989 = CARTESIAN_POINT ( 'NONE',  ( 2.844419195333417250, 64.07772472696797195, -13.19709045098189826 ) ) ;
#990 = CARTESIAN_POINT ( 'NONE',  ( 13.16029344000198620, 42.53708686388746685, -3.020864121732791396 ) ) ;
#991 = CARTESIAN_POINT ( 'NONE',  ( 12.52796351933140429, 39.24719058125410953, 5.030018464370217046 ) ) ;
#992 = ORIENTED_EDGE ( 'NONE', *, *, #16917, .F. ) ;
#993 = CARTESIAN_POINT ( 'NONE',  ( -8.704689286822198113, 70.51503155829134073, -10.32237615012925858 ) ) ;
#994 = CARTESIAN_POINT ( 'NONE',  ( -9.897107763165278627, 61.57380692958660262, -9.182555981961492364 ) ) ;
#995 = CARTESIAN_POINT ( 'NONE',  ( 9.520470885617715595, 2.129999999999992788, 6.917026985038135400 ) ) ;
#996 = ORIENTED_EDGE ( 'NONE', *, *, #2626, .F. ) ;
#997 = CARTESIAN_POINT ( 'NONE',  ( -8.167758447988427761, 40.49042146826998589, -10.74885325159674565 ) ) ;
#998 = ORIENTED_EDGE ( 'NONE', *, *, #4773, .T. ) ;
#999 = CARTESIAN_POINT ( 'NONE',  ( 2.621994543952811015E-15, 25.17999999999999616, -14.19474002721660355 ) ) ;
#1000 = CARTESIAN_POINT ( 'NONE',  ( 18.62500000000000000, -83.24999999999980105, 1.560692158462880521E-12 ) ) ;
#1001 = DIRECTION ( 'NONE',  ( -1.000000000000000000, 0.000000000000000000, 0.000000000000000000 ) ) ;
#1002 = VECTOR ( 'NONE', #7762, 1000.000000000000000 ) ;
#1003 = CARTESIAN_POINT ( 'NONE',  ( 13.39390915008829630, 57.37105770510941483, 1.689157604109823074 ) ) ;
#1004 = CARTESIAN_POINT ( 'NONE',  ( 12.20311627183846959, 78.64184583226609959, -5.773582477899624976 ) ) ;
#1005 = CARTESIAN_POINT ( 'NONE',  ( -7.272992578804310604, 75.37999999999999545, 10.01041549318726709 ) ) ;
#1006 = CARTESIAN_POINT ( 'NONE',  ( -13.50000000000000000, 36.92999999999999972, -3.306546357697853733E-15 ) ) ;
#1007 = CARTESIAN_POINT ( 'NONE',  ( 3.636496289402154414, 75.83000000000001251, 11.19198476289190936 ) ) ;
#1008 = CARTESIAN_POINT ( 'NONE',  ( -1.403940416332137451E-13, 0.000000000000000000, 19.99999999999999289 ) ) ;
#1009 = CARTESIAN_POINT ( 'NONE',  ( 8.047696313746376617, -99.99999999999994316, 9.235391612970973441 ) ) ;
#1010 = DIRECTION ( 'NONE',  ( 0.000000000000000000, 0.000000000000000000, 1.000000000000000000 ) ) ;
#1011 = CARTESIAN_POINT ( 'NONE',  ( 11.37500000000000178, -75.99999999999980105, 9.531744055041752924E-13 ) ) ;
#1012 = CARTESIAN_POINT ( 'NONE',  ( 15.58845726811984811, 0.000000000000000000, 11.00000000000007283 ) ) ;
#1013 = CARTESIAN_POINT ( 'NONE',  ( 9.827588045523224736, 33.78981817295442625, -9.258195743607105399 ) ) ;
#1014 = CARTESIAN_POINT ( 'NONE',  ( -13.48486571972425274, 73.90797088387792257, -0.6398426247094320951 ) ) ;
#1015 = ORIENTED_EDGE ( 'NONE', *, *, #14814, .T. ) ;
#1016 = ORIENTED_EDGE ( 'NONE', *, *, #3206, .T. ) ;
#1017 =( BOUNDED_CURVE ( )  B_SPLINE_CURVE ( 2, ( #15588, #5906, #8648, #13915, #8735, #6084, #14094, #11285, #16662, #671, #3228 ),
 .UNSPECIFIED., .F., .F. ) 
 B_SPLINE_CURVE_WITH_KNOTS ( ( 3, 2, 2, 2, 2, 3 ),
 ( 0.4616868741582292324, 0.4666666666666666741, 0.4722222222222222099, 0.4777777777777778012, 0.4833333333333333370, 0.4861111111111111049 ),
 .UNSPECIFIED. ) 
 CURVE ( )  GEOMETRIC_REPRESENTATION_ITEM ( )  RATIONAL_B_SPLINE_CURVE ( ( 0.9909066287976675547, 0.9561288891717594218, 1.000000000000000000, 0.9510565162951535312, 1.000000000000000000, 0.9510565162951535312, 1.000000000000000000, 0.9510565162951535312, 1.000000000000000000, 0.9755282581475768211, 0.9755282581475768211 ) ) 
 REPRESENTATION_ITEM ( '' )  );
#1018 = CARTESIAN_POINT ( 'NONE',  ( -7.499999999999998224, -8.000000000000000000, -22.50000000000000355 ) ) ;
#1019 = ORIENTED_EDGE ( 'NONE', *, *, #6979, .F. ) ;
#1020 = CARTESIAN_POINT ( 'NONE',  ( -10.92172942406178926, 13.63000000000000256, -7.935100905948389460 ) ) ;
#1021 = CARTESIAN_POINT ( 'NONE',  ( -11.37499999999999645, -48.87499999999990052, -9.545674412382054647E-13 ) ) ;
#1022 = CARTESIAN_POINT ( 'NONE',  ( -4.783579317106955386, 44.50765774798735919, 12.62540879120737536 ) ) ;
#1023 = CARTESIAN_POINT ( 'NONE',  ( -7.500000000000000000, 98.93000000000002103, 9.000000000000000000 ) ) ;
#1024 = CARTESIAN_POINT ( 'NONE',  ( 9.116104188755297599, 66.82557654486986110, -9.969699158624095503 ) ) ;
#1025 = VECTOR ( 'NONE', #3269, 1000.000000000000000 ) ;
#1026 = CARTESIAN_POINT ( 'NONE',  ( -4.171729424061791036, 50.53000000000000114, 12.83926296998457239 ) ) ;
#1027 = CARTESIAN_POINT ( 'NONE',  ( -5.791868581402612293, 71.46924316949180422, 12.19443570704414093 ) ) ;
#1028 = CARTESIAN_POINT ( 'NONE',  ( 7.714727599197338748, -96.77812499999976126, 18.62500000000063949 ) ) ;
#1029 = CARTESIAN_POINT ( 'NONE',  ( -1.270456549871447738, 68.63430995385745348, 13.44010555243231053 ) ) ;
#1030 = CARTESIAN_POINT ( 'NONE',  ( -13.16986379960055231, -77.00624999999982379, 13.16986379959834252 ) ) ;
#1031 = EDGE_CURVE ( 'NONE', #4554, #3828, #15695, .T. ) ;
#1032 = CARTESIAN_POINT ( 'NONE',  ( 4.606558825016942471, 55.01407570091451760, -12.68986247441658932 ) ) ;
#1033 = CARTESIAN_POINT ( 'NONE',  ( 7.272992578804308828, 19.98000000000000043, 10.01041549318726709 ) ) ;
#1034 = CARTESIAN_POINT ( 'NONE',  ( -7.714727599197335195, -21.85312499999995239, -18.62500000000064304 ) ) ;
#1035 = AXIS2_PLACEMENT_3D ( 'NONE', #6946, #16466, #10917 ) ;
#1036 = CARTESIAN_POINT ( 'NONE',  ( -1.945342937830138563, 65.61008263105732397, 13.36017202698423922 ) ) ;
#1037 = CARTESIAN_POINT ( 'NONE',  ( -8.512854481965995035, 62.35381330728030491, 10.47804304773685224 ) ) ;
#1038 = CARTESIAN_POINT ( 'NONE',  ( -8.740105143331430071, 35.34338649247177955, 10.29126063676346980 ) ) ;
#1039 = CARTESIAN_POINT ( 'NONE',  ( -2.919924463492937772, 40.28498943413073619, -13.18046540264134237 ) ) ;
#1040 = CARTESIAN_POINT ( 'NONE',  ( -13.49990871899026601, 31.94501881797403442, 0.4409628020136921456 ) ) ;
#1041 = DIRECTION ( 'NONE',  ( 0.000000000000000000, 1.000000000000000000, 0.000000000000000000 ) ) ;
#1042 = CARTESIAN_POINT ( 'NONE',  ( 8.139855941678256102, 59.98916145259055099, 10.77923023974760497 ) ) ;
#1043 = CARTESIAN_POINT ( 'NONE',  ( 8.343458848123578520, -8.020000000000003126, 11.48378591275254124 ) ) ;
#1044 = CARTESIAN_POINT ( 'NONE',  ( -1.412718313214967214, 53.62924654513680878, 13.42809310199930728 ) ) ;
#1045 = CARTESIAN_POINT ( 'NONE',  ( 7.272992578804308828, 54.98000000000000398, 10.01041549318726709 ) ) ;
#1046 = CARTESIAN_POINT ( 'NONE',  ( 10.92172942406179104, 77.73000000000000398, -7.935100905948385908 ) ) ;
#1047 = CARTESIAN_POINT ( 'NONE',  ( 11.44877280849391532, 51.69754644816881495, -7.157341881666669181 ) ) ;
#1048 = CARTESIAN_POINT ( 'NONE',  ( -12.56737935825091945, 38.10897242895168802, 4.930623318646805586 ) ) ;
#1049 = EDGE_CURVE ( 'NONE', #17099, #6127, #17123, .T. ) ;
#1050 = CARTESIAN_POINT ( 'NONE',  ( 11.88911771378908711, 36.66659916247261464, -6.395327377679192793 ) ) ;
#1051 = CARTESIAN_POINT ( 'NONE',  ( -11.37500000000039613, -49.91562499999989910, 4.711679271993000739 ) ) ;
#1052 = CARTESIAN_POINT ( 'NONE',  ( -0.3656471757371563269, 74.66685158956377677, 13.49665596708117654 ) ) ;
#1053 = CARTESIAN_POINT ( 'NONE',  ( -12.11600929618134970, 77.14899403401574318, 5.954317193221099203 ) ) ;
#1054 = DIRECTION ( 'NONE',  ( 1.426480712616743731E-14, 0.000000000000000000, -1.000000000000000000 ) ) ;
#1055 = CARTESIAN_POINT ( 'NONE',  ( 7.499999999999999112, 108.3824470675415341, 4.067225351102826458 ) ) ;
#1056 = ORIENTED_EDGE ( 'NONE', *, *, #8622, .T. ) ;
#1057 = CARTESIAN_POINT ( 'NONE',  ( 11.76794919243112325, 8.429999999999992610, 1.734723475976807094E-15 ) ) ;
#1058 = ORIENTED_EDGE ( 'NONE', *, *, #12188, .F. ) ;
#1059 = CARTESIAN_POINT ( 'NONE',  ( 11.76794919243112325, 55.42999999999999972, 1.441158131103945434E-15 ) ) ;
#1060 = CARTESIAN_POINT ( 'NONE',  ( 4.711679271993006957, -89.52812499999977547, 11.37500000000039613 ) ) ;
#1061 = CARTESIAN_POINT ( 'NONE',  ( 13.50000000000000355, 56.57999999999999829, -4.386415899144233244 ) ) ;
#1062 = CARTESIAN_POINT ( 'NONE',  ( 4.171729424061791924, -4.969999999999995310, -12.83926296998457239 ) ) ;
#1063 = CARTESIAN_POINT ( 'NONE',  ( 10.58057089751780566, 75.74942444919939533, -8.384628530423594128 ) ) ;
#1064 = DIRECTION ( 'NONE',  ( -1.000000000000000000, -0.000000000000000000, -0.000000000000000000 ) ) ;
#1065 = CARTESIAN_POINT ( 'NONE',  ( 3.041627741621593994, 65.78941339898256047, 13.15297391146506101 ) ) ;
#1066 = CARTESIAN_POINT ( 'NONE',  ( 10.92172942406179104, 75.73000000000000398, -7.935100905948385908 ) ) ;
#1067 = CARTESIAN_POINT ( 'NONE',  ( 9.520470885617715595, 40.12999999999999545, 6.917026985038134512 ) ) ;
#1068 = DIRECTION ( 'NONE',  ( 0.000000000000000000, -1.000000000000000000, 0.000000000000000000 ) ) ;
#1069 = CARTESIAN_POINT ( 'NONE',  ( -9.927680929899530327, 59.28455817258709004, 9.148293018334287652 ) ) ;
#1070 = CARTESIAN_POINT ( 'NONE',  ( 12.47446446985702906, 45.24145293083233810, 5.182912669380336013 ) ) ;
#1071 = CARTESIAN_POINT ( 'NONE',  ( 13.35909562912327608, 69.36166794184582329, 1.954686695093853732 ) ) ;
#1072 = DIRECTION ( 'NONE',  ( -0.000000000000000000, -1.000000000000000000, -0.000000000000000000 ) ) ;
#1073 = CARTESIAN_POINT ( 'NONE',  ( 12.05249706929546072, 30.65406261480569583, -6.081942500887944192 ) ) ;
#1074 = CARTESIAN_POINT ( 'NONE',  ( -7.530017562689784505, 55.46222776646441588, -11.20493419439256755 ) ) ;
#1075 = CARTESIAN_POINT ( 'NONE',  ( -13.48049505424421568, 49.90497277773586404, -0.7254708853913678368 ) ) ;
#1076 = CARTESIAN_POINT ( 'NONE',  ( 9.418187565439815501, 63.81058986697370017, -9.677497028817999336 ) ) ;
#1077 = CARTESIAN_POINT ( 'NONE',  ( 12.45500488473927092, 42.62014939293063520, -5.223402740974586678 ) ) ;
#1078 = CARTESIAN_POINT ( 'NONE',  ( 12.50570607633773967, 39.24506257281584709, 5.085017721920233491 ) ) ;
#1079 = AXIS2_PLACEMENT_3D ( 'NONE', #1741, #4228, #11215 ) ;
#1080 = ORIENTED_EDGE ( 'NONE', *, *, #8622, .F. ) ;
#1081 = CARTESIAN_POINT ( 'NONE',  ( -9.879805435650132139, 70.57295972474388179, -9.199969855269857888 ) ) ;
#1082 = CARTESIAN_POINT ( 'NONE',  ( -10.11877999215449542, 61.58546918468492493, -8.936496873947890052 ) ) ;
#1083 = CARTESIAN_POINT ( 'NONE',  ( -11.76794919243112325, 3.930000000000002824, -2.602085213965210642E-15 ) ) ;
#1084 = ORIENTED_EDGE ( 'NONE', *, *, #10622, .T. ) ;
#1085 = ORIENTED_EDGE ( 'NONE', *, *, #13634, .F. ) ;
#1086 = CARTESIAN_POINT ( 'NONE',  ( 10.92172942406179104, 21.73000000000000043, -7.935100905948385908 ) ) ;
#1087 = CARTESIAN_POINT ( 'NONE',  ( 18.62499999999934630, -65.55937499999984652, 7.714727599200467800 ) ) ;
#1088 = CARTESIAN_POINT ( 'NONE',  ( 2.852439471677590710, 61.07744184195599502, -13.19548016026537773 ) ) ;
#1089 = CARTESIAN_POINT ( 'NONE',  ( 13.38817278408007105, 57.36945051200932966, 1.734111481910428409 ) ) ;
#1090 = EDGE_CURVE ( 'NONE', #902, #15411, #10862, .T. ) ;
#1091 = CARTESIAN_POINT ( 'NONE',  ( 11.76794919243112680, 67.57999999999998408, -3.823638476888993942 ) ) ;
#1092 = CARTESIAN_POINT ( 'NONE',  ( 11.76794919243112325, 73.42999999999999261, 1.441158131103945434E-15 ) ) ;
#1093 = CARTESIAN_POINT ( 'NONE',  ( 5.441113646577480978, 5.918584287042170544, -25.42428528562854595 ) ) ;
#1094 = AXIS2_PLACEMENT_3D ( 'NONE', #11321, #3086, #15360 ) ;
#1095 = CARTESIAN_POINT ( 'NONE',  ( 2.445080149700053643E-15, 42.17999999999999261, -13.50000000000000000 ) ) ;
#1096 = CARTESIAN_POINT ( 'NONE',  ( 3.122018999846114085, 10.00000000000000000, -13.05075980765145438 ) ) ;
#1097 = CARTESIAN_POINT ( 'NONE',  ( -9.552639591052204498E-13, -12.48749999999997051, 11.37500000000000000 ) ) ;
#1098 = CARTESIAN_POINT ( 'NONE',  ( 7.500000000000000888, 98.93000000000002103, 9.000000000000000000 ) ) ;
#1099 = CARTESIAN_POINT ( 'NONE',  ( -2.522983078673279752E-14, 34.17999999999999972, -13.50000000000000000 ) ) ;
#1100 = CARTESIAN_POINT ( 'NONE',  ( -8.446523378668436166, 73.50299463280887835, -10.53513265744836502 ) ) ;
#1101 = ORIENTED_EDGE ( 'NONE', *, *, #3547, .F. ) ;
#1102 = ORIENTED_EDGE ( 'NONE', *, *, #4492, .T. ) ;
#1103 = CARTESIAN_POINT ( 'NONE',  ( 9.520470885617717371, 79.72999999999998977, -6.917026985038131848 ) ) ;
#1104 = ORIENTED_EDGE ( 'NONE', *, *, #15443, .T. ) ;
#1105 = CARTESIAN_POINT ( 'NONE',  ( -8.043339635997652337, -100.9062499999997868, 8.043339635996300530 ) ) ;
#1106 = AXIS2_PLACEMENT_3D ( 'NONE', #10248, #3509, #12716 ) ;
#1107 = CARTESIAN_POINT ( 'NONE',  ( -8.267728653884569567, 44.36549807078887397, 10.69103896247519003 ) ) ;
#1108 = CARTESIAN_POINT ( 'NONE',  ( -7.499999999999995559, -27.00941661075429323, 5.548846425319426956 ) ) ;
#1109 = CARTESIAN_POINT ( 'NONE',  ( 9.716038052031565897, 66.79547513456357422, -9.373145993641442075 ) ) ;
#1110 = EDGE_CURVE ( 'NONE', #10472, #4018, #13395, .T. ) ;
#1111 = CARTESIAN_POINT ( 'NONE',  ( 2.607531440858944223E-15, 55.17999999999998550, -14.19474002721660355 ) ) ;
#1112 = CARTESIAN_POINT ( 'NONE',  ( -11.83577994726966054, 71.17054626581648336, 6.493405617986467426 ) ) ;
#1113 = PRODUCT_DEFINITION_SHAPE ( 'NONE', 'NONE',  #17488 ) ;
#1114 = CIRCLE ( 'NONE', #11015, 26.00000000000000355 ) ;
#1115 = CARTESIAN_POINT ( 'NONE',  ( -18.62500000000064659, -92.61562499999978115, 7.714727599197335195 ) ) ;
#1116 = CARTESIAN_POINT ( 'NONE',  ( -13.42211799135032990, 67.98038489383687022, 1.448088636224807102 ) ) ;
#1117 = CARTESIAN_POINT ( 'NONE',  ( 13.16986379959833897, -7.318749999999964118, 13.16986379960055409 ) ) ;
#1118 = CARTESIAN_POINT ( 'NONE',  ( 0.000000000000000000, 9.999999999999998224, 0.000000000000000000 ) ) ;
#1119 = CARTESIAN_POINT ( 'NONE',  ( 7.272992578804311492, 20.87999999999999545, -10.01041549318726709 ) ) ;
#1120 = CARTESIAN_POINT ( 'NONE',  ( 13.16986379960055054, -85.33124999999978400, -13.16986379959834430 ) ) ;
#1121 = CARTESIAN_POINT ( 'NONE',  ( -13.38213899561058895, 64.99218069301205958, 1.780040424083840556 ) ) ;
#1122 = CARTESIAN_POINT ( 'NONE',  ( -4.052283961879332708, 35.53437198618238568, 12.87817188429518467 ) ) ;
#1123 = ORIENTED_EDGE ( 'NONE', *, *, #10137, .T. ) ;
#1124 = CARTESIAN_POINT ( 'NONE',  ( -11.76794919243112325, 32.77999999999999403, -3.823638476888998827 ) ) ;
#1125 = CARTESIAN_POINT ( 'NONE',  ( 0.000000000000000000, 73.00000000000001421, 0.000000000000000000 ) ) ;
#1126 = CARTESIAN_POINT ( 'NONE',  ( 3.636496289402157078, 27.02999999999999758, -11.19198476289190936 ) ) ;
#1127 = CARTESIAN_POINT ( 'NONE',  ( -3.203942090712391888, 31.29520102517548708, -13.11476468382334737 ) ) ;
#1128 = DIRECTION ( 'NONE',  ( 0.000000000000000000, 0.000000000000000000, -1.000000000000000000 ) ) ;
#1129 = CARTESIAN_POINT ( 'NONE',  ( 11.65241955595561585, 60.17635480250425672, 6.816973529922489838 ) ) ;
#1130 = EDGE_CURVE ( 'NONE', #10403, #10678, #7750, .T. ) ;
#1131 = CARTESIAN_POINT ( 'NONE',  ( 13.50000000000000000, -7.570000000000000284, 1.734723475976807094E-15 ) ) ;
#1132 = CARTESIAN_POINT ( 'NONE',  ( -6.089806512862788956, 53.45753655534689841, 12.05607447093654017 ) ) ;
#1133 = CARTESIAN_POINT ( 'NONE',  ( 2.272985001014427788E-15, 53.17999999999999972, -12.37355403259654985 ) ) ;
#1134 = CARTESIAN_POINT ( 'NONE',  ( 13.49999999999999822, 77.27999999999998693, 4.386415899144237684 ) ) ;
#1135 = CARTESIAN_POINT ( 'NONE',  ( 11.00335429800770548, 51.13480760581911255, 7.825213182322699801 ) ) ;
#1136 = CARTESIAN_POINT ( 'NONE',  ( -9.597058931428728457, 37.55844031602762101, -9.501180398282993878 ) ) ;
#1137 = CARTESIAN_POINT ( 'NONE',  ( 13.35040085901588824, 36.35962275902586072, 2.008008797607404361 ) ) ;
#1138 = CARTESIAN_POINT ( 'NONE',  ( 9.538709233711902776E-13, -61.36249999999986215, -11.37499999999999645 ) ) ;
#1139 = CARTESIAN_POINT ( 'NONE',  ( -5.988508216935491291, 74.46151138467401154, 12.09920782539440154 ) ) ;
#1140 = CARTESIAN_POINT ( 'NONE',  ( -12.09693526138493525, 77.15052554825793152, 5.992971486588084318 ) ) ;
#1141 = CARTESIAN_POINT ( 'NONE',  ( -12.98374536458790196, 79.79765901695760988, -3.704304229944536786 ) ) ;
#1142 = CARTESIAN_POINT ( 'NONE',  ( -3.636496289402156190, 13.53000000000001357, 11.19198476289190758 ) ) ;
#1143 = CARTESIAN_POINT ( 'NONE',  ( 7.499999999999999112, 106.5829119071944717, 7.723695278929457508 ) ) ;
#1144 = ORIENTED_EDGE ( 'NONE', *, *, #3312, .F. ) ;
#1145 = CARTESIAN_POINT ( 'NONE',  ( 7.272992578804311492, 2.880000000000001670, -10.01041549318726709 ) ) ;
#1146 = ORIENTED_EDGE ( 'NONE', *, *, #15825, .T. ) ;
#1147 = CARTESIAN_POINT ( 'NONE',  ( -9.520470885617715595, 53.62999999999999545, -6.917026985038136289 ) ) ;
#1148 = CARTESIAN_POINT ( 'NONE',  ( -8.043339635997654113, -53.10624999999986073, 8.043339635996304082 ) ) ;
#1149 = CARTESIAN_POINT ( 'NONE',  ( 13.16986379960055054, -18.73124999999995666, -13.16986379959834430 ) ) ;
#1150 = CARTESIAN_POINT ( 'NONE',  ( -8.343458848123576743, -4.520000000000004903, -11.48378591275254301 ) ) ;
#1151 = CARTESIAN_POINT ( 'NONE',  ( 6.051126895917462001, 75.95900626949409684, -12.06810164290940968 ) ) ;
#1152 = EDGE_CURVE ( 'NONE', #3134, #1210, #16777, .T. ) ;
#1153 = PLANE ( 'NONE',  #8823 ) ;
#1154 = CARTESIAN_POINT ( 'NONE',  ( 0.3314664981419376266, 65.69191830627838158, 13.49594832441332670 ) ) ;
#1155 = CARTESIAN_POINT ( 'NONE',  ( -4.171729424061791036, 68.53000000000000114, 12.83926296998457239 ) ) ;
#1156 = CARTESIAN_POINT ( 'NONE',  ( -11.76794919243112325, 42.08000000000000540, 3.823638476888994386 ) ) ;
#1157 = CARTESIAN_POINT ( 'NONE',  ( 0.000000000000000000, 80.93000000000000682, -13.50000000000000000 ) ) ;
#1158 = CARTESIAN_POINT ( 'NONE',  ( -12.86588924449608484, 58.78300137090919009, -4.092555612934534182 ) ) ;
#1159 = CARTESIAN_POINT ( 'NONE',  ( 12.95119434482599630, 45.29360578691247952, 3.810224031054839422 ) ) ;
#1160 = CARTESIAN_POINT ( 'NONE',  ( 12.58190901537911977, 69.60887662769496842, -4.936570319405274354 ) ) ;
#1161 = CYLINDRICAL_SURFACE ( 'NONE', #15110, 26.00000000000000355 ) ;
#1162 = LINE ( 'NONE', #9576, #6487 ) ;
#1163 = CARTESIAN_POINT ( 'NONE',  ( -10.10275593513610737, 55.58463057449298361, -8.954572238356126590 ) ) ;
#1164 = CARTESIAN_POINT ( 'NONE',  ( -13.46222882471981741, 49.96493226193709347, 1.009247901310075690 ) ) ;
#1165 = CARTESIAN_POINT ( 'NONE',  ( 11.27120675886632029, 63.70861490660946203, -7.431139975753272786 ) ) ;
#1166 = CARTESIAN_POINT ( 'NONE',  ( 7.715407790152941203, 42.88976810797701233, -11.08212475357666449 ) ) ;
#1167 = CARTESIAN_POINT ( 'NONE',  ( 12.58936429392694301, 39.25315851018460478, 4.875368239649940705 ) ) ;
#1168 = VERTEX_POINT ( 'NONE', #1555 ) ;
#1169 = CARTESIAN_POINT ( 'NONE',  ( -11.69253541478880720, 70.67755481803949635, -6.804811722709197319 ) ) ;
#1170 = CARTESIAN_POINT ( 'NONE',  ( -3.338982230527045569, 61.29999130979701505, -13.08671784421840023 ) ) ;
#1171 = CARTESIAN_POINT ( 'NONE',  ( 11.76794919243112325, 2.280000000000006466, 3.823638476888996163 ) ) ;
#1172 = VERTEX_POINT ( 'NONE', #415 ) ;
#1173 = ORIENTED_EDGE ( 'NONE', *, *, #13007, .F. ) ;
#1174 = CARTESIAN_POINT ( 'NONE',  ( -13.49999999999999822, 20.08000000000001251, 4.386415899144235908 ) ) ;
#1175 = CARTESIAN_POINT ( 'NONE',  ( -13.16986379960055231, -77.00624999999982379, 13.16986379959834252 ) ) ;
#1176 = CARTESIAN_POINT ( 'NONE',  ( 3.934034384636251325, 61.03850454420580007, -12.91965331869873346 ) ) ;
#1177 = EDGE_CURVE ( 'NONE', #17275, #8372, #10142, .T. ) ;
#1178 = CARTESIAN_POINT ( 'NONE',  ( 7.656218467254686466, 71.96771731040691122, 11.11903937377953611 ) ) ;
#1179 = CARTESIAN_POINT ( 'NONE',  ( 13.42377694829353985, 57.38002766246249564, 1.436435505632925658 ) ) ;
#1180 = CARTESIAN_POINT ( 'NONE',  ( 11.76794919243112325, 73.27999999999998693, 3.823638476888996607 ) ) ;
#1181 = CARTESIAN_POINT ( 'NONE',  ( -7.272992578804310604, 81.38000000000000966, 10.01041549318726709 ) ) ;
#1182 = CARTESIAN_POINT ( 'NONE',  ( -9.886435270270100162, 47.28669829188292795, 9.192848475936937547 ) ) ;
#1183 = PRODUCT_DEFINITION_CONTEXT ( 'detailed design', #1448, 'design' ) ;
#1184 = CARTESIAN_POINT ( 'NONE',  ( -8.891200544363830713E-16, 37.67999999999999261, 13.50000000000000000 ) ) ;
#1185 = CARTESIAN_POINT ( 'NONE',  ( -0.2535909892785384590, 9.999999999999994671, -13.17844121984262173 ) ) ;
#1186 = CARTESIAN_POINT ( 'NONE',  ( 11.37499999999960210, -32.25937499999992042, 4.711679271994918317 ) ) ;
#1187 = CARTESIAN_POINT ( 'NONE',  ( 7.347880794884122694E-16, 0.000000000000000000, -20.00000000000000000 ) ) ;
#1188 = CARTESIAN_POINT ( 'NONE',  ( 4.369696808009779332, 34.02284990421056676, -12.77326014878184424 ) ) ;
#1189 = CARTESIAN_POINT ( 'NONE',  ( -4.416228722299345044, 73.33875342350749804, -12.76045521491836432 ) ) ;
#1190 = ORIENTED_EDGE ( 'NONE', *, *, #13167, .F. ) ;
#1191 = VERTEX_POINT ( 'NONE', #11032 ) ;
#1192 = CARTESIAN_POINT ( 'NONE',  ( 9.520470885617717371, 73.73000000000000398, -6.917026985038131848 ) ) ;
#1193 = VERTEX_POINT ( 'NONE', #16404 ) ;
#1194 = AXIS2_PLACEMENT_3D ( 'NONE', #10, #4075, #8337 ) ;
#1195 = CARTESIAN_POINT ( 'NONE',  ( -4.711679271994915652, -101.9468749999997783, 11.37499999999960210 ) ) ;
#1196 = CARTESIAN_POINT ( 'NONE',  ( -10.12244397357995140, 44.27432646096063706, 8.932308212114547175 ) ) ;
#1197 = CARTESIAN_POINT ( 'NONE',  ( 10.85009556066085423, 7.815224736851130949, 15.50190989971483191 ) ) ;
#1198 = CARTESIAN_POINT ( 'NONE',  ( -4.171729424061787483, 40.32999999999999829, -12.83926296998457417 ) ) ;
#1199 = CARTESIAN_POINT ( 'NONE',  ( -11.83839496929498125, 71.17035886798730360, 6.488638129243179620 ) ) ;
#1200 = VECTOR ( 'NONE', #2937, 1000.000000000000000 ) ;
#1201 = CARTESIAN_POINT ( 'NONE',  ( -18.62499999999934985, -73.88437499999982094, -7.714727599200458918 ) ) ;
#1202 = CARTESIAN_POINT ( 'NONE',  ( -11.66904316095729222, 68.18248099459721345, 6.788478734277004989 ) ) ;
#1203 = CARTESIAN_POINT ( 'NONE',  ( -7.714727599197334307, -31.25312499999991545, -18.62500000000064659 ) ) ;
#1204 = CARTESIAN_POINT ( 'NONE',  ( 3.111368884622620623, 55.06813134461953751, -13.13662995333488226 ) ) ;
#1205 = CARTESIAN_POINT ( 'NONE',  ( -7.409984580736203970E-16, 16.68000000000000327, 12.37355403259654985 ) ) ;
#1206 = DIRECTION ( 'NONE',  ( 1.000000000000000000, 8.673617379884039170E-17, -0.000000000000000000 ) ) ;
#1207 = ADVANCED_FACE ( 'NONE', ( #6254 ), #4748, .F. ) ;
#1208 = CARTESIAN_POINT ( 'NONE',  ( -13.34368233115651492, 65.00195984828552298, 2.053198378037492056 ) ) ;
#1209 = CARTESIAN_POINT ( 'NONE',  ( -7.063482594716048446, 35.41767491092237918, 11.50466891869187691 ) ) ;
#1210 = VERTEX_POINT ( 'NONE', #13050 ) ;
#1211 = CARTESIAN_POINT ( 'NONE',  ( -15.58845726811999910, 0.000000000000000000, 10.99999999999985256 ) ) ;
#1212 = CARTESIAN_POINT ( 'NONE',  ( -8.029972511114698008, 31.48422938242913105, -10.85219181568965929 ) ) ;
#1213 = CARTESIAN_POINT ( 'NONE',  ( 15.28534784291390203, 6.548267719634619510, 18.06260399879755951 ) ) ;
#1214 = CARTESIAN_POINT ( 'NONE',  ( -3.636496289402152637, -11.66999999999999993, -11.19198476289190936 ) ) ;
#1215 = CARTESIAN_POINT ( 'NONE',  ( 5.573835160001226363, 59.88200068511800822, 12.30730957908311751 ) ) ;
#1216 = CARTESIAN_POINT ( 'NONE',  ( 2.621994543952811015E-15, -9.820000000000003837, -14.19474002721660355 ) ) ;
#1217 = CARTESIAN_POINT ( 'NONE',  ( -7.325695255518703597, 53.40656810623330131, 11.33985798352976992 ) ) ;
#1218 = CARTESIAN_POINT ( 'NONE',  ( -7.576616670048093940E-16, 51.68000000000000682, 12.37355403259654985 ) ) ;
#1219 = CARTESIAN_POINT ( 'NONE',  ( -13.49999999999999822, 67.07999999999999829, 4.386415899144235908 ) ) ;
#1220 = CARTESIAN_POINT ( 'NONE',  ( 5.686689245591225905, 50.88656960456093259, 12.25087184074811120 ) ) ;
#1221 = CARTESIAN_POINT ( 'NONE',  ( -10.20473357957621197, 37.59009158050992738, -8.838276559641728980 ) ) ;
#1222 = CARTESIAN_POINT ( 'NONE',  ( 9.231307355299586348, 36.04034459707229132, 9.850538178411547108 ) ) ;
#1223 = CARTESIAN_POINT ( 'NONE',  ( -8.043339635997652337, -84.25624999999980957, 8.043339635996300530 ) ) ;
#1224 = EDGE_CURVE ( 'NONE', #6427, #1193, #9016, .T. ) ;
#1225 = CARTESIAN_POINT ( 'NONE',  ( -6.087077674780319470, 74.45759876751071715, 12.04979220636686144 ) ) ;
#1226 = CARTESIAN_POINT ( 'NONE',  ( -12.47207658550254905, 76.74188438275474766, -5.167046129524251796 ) ) ;
#1227 = CARTESIAN_POINT ( 'NONE',  ( -10.97791022018516394, 79.63287582280005950, -7.869652631373966756 ) ) ;
#1228 = CARTESIAN_POINT ( 'NONE',  ( 0.000000000000000000, 102.9300000000000068, 0.000000000000000000 ) ) ;
#1229 = CARTESIAN_POINT ( 'NONE',  ( -7.409984580736203970E-16, 4.680000000000003268, 12.37355403259654985 ) ) ;
#1230 = CARTESIAN_POINT ( 'NONE',  ( -11.76794919243112325, 51.07999999999999829, 3.823638476888994830 ) ) ;
#1231 = CARTESIAN_POINT ( 'NONE',  ( 4.711679271993006957, -56.22812499999984936, 11.37500000000039613 ) ) ;
#1232 = CARTESIAN_POINT ( 'NONE',  ( 2.138189814981843906, 9.756881417667548462, 13.50000004204441062 ) ) ;
#1233 = CARTESIAN_POINT ( 'NONE',  ( 13.49999999999999822, -11.72000000000000064, 4.386415899144237684 ) ) ;
#1234 = CARTESIAN_POINT ( 'NONE',  ( -9.999999999999776179, 0.000000000000000000, -17.32050807568890605 ) ) ;
#1235 = CARTESIAN_POINT ( 'NONE',  ( 8.595313431481731214, 75.84998225435066388, -10.41012029664250349 ) ) ;
#1236 = DIRECTION ( 'NONE',  ( -0.5000000000000074385, 0.000000000000000000, 0.8660254037844342667 ) ) ;
#1237 = CARTESIAN_POINT ( 'NONE',  ( 9.520470885617717371, 43.72999999999999687, -6.917026985038131848 ) ) ;
#1238 = CARTESIAN_POINT ( 'NONE',  ( -12.52061518882791269, 41.11351867588017228, 5.048379448138805792 ) ) ;
#1239 = CARTESIAN_POINT ( 'NONE',  ( -8.868632591895519113, 58.52285990151153783, -10.17867040326453143 ) ) ;
#1240 = CARTESIAN_POINT ( 'NONE',  ( 0.000000000000000000, 102.9300000000000068, 0.000000000000000000 ) ) ;
#1241 = CARTESIAN_POINT ( 'NONE',  ( 0.000000000000000000, 5.918584287042170544, 0.000000000000000000 ) ) ;
#1242 = LINE ( 'NONE', #14668, #12967 ) ;
#1243 = CARTESIAN_POINT ( 'NONE',  ( -0.5643014959054915014, 55.20029019360543998, -13.48820175703197677 ) ) ;
#1244 = ADVANCED_FACE ( 'NONE', ( #9982 ), #16343, .T. ) ;
#1245 = CARTESIAN_POINT ( 'NONE',  ( -13.25473226480498035, 49.83966860457066161, -2.561852220214583919 ) ) ;
#1246 = CARTESIAN_POINT ( 'NONE',  ( 10.70554398665652585, 63.74254191304165573, -8.236043843619819782 ) ) ;
#1247 = CARTESIAN_POINT ( 'NONE',  ( 10.11861299488508514, 42.77454474994834754, -8.937100350925991421 ) ) ;
#1248 = CARTESIAN_POINT ( 'NONE',  ( 13.22408915331992674, 39.33228484707264272, 2.764232869092419609 ) ) ;
#1249 = ORIENTED_EDGE ( 'NONE', *, *, #6676, .T. ) ;
#1250 = CARTESIAN_POINT ( 'NONE',  ( -12.90681428308145939, 70.78796989954061303, -3.960305618596332788 ) ) ;
#1251 = CARTESIAN_POINT ( 'NONE',  ( 11.37500000000039435, -17.69062499999995808, -4.711679271993003404 ) ) ;
#1252 = VERTEX_POINT ( 'NONE', #3584 ) ;
#1253 = ORIENTED_EDGE ( 'NONE', *, *, #3103, .F. ) ;
#1254 = CARTESIAN_POINT ( 'NONE',  ( -4.171729424061787483, 19.33000000000001251, -12.83926296998457417 ) ) ;
#1255 = CARTESIAN_POINT ( 'NONE',  ( 7.999999999999904965, 7.773118517290098950, 17.32050807568881368 ) ) ;
#1256 = CARTESIAN_POINT ( 'NONE',  ( 6.434165136549590436, 47.91625709899204821, 11.86847022325157752 ) ) ;
#1257 = CARTESIAN_POINT ( 'NONE',  ( 13.50000000000000355, 13.57999999999999652, -4.386415899144233244 ) ) ;
#1258 = CARTESIAN_POINT ( 'NONE',  ( 2.397323522673310947, 71.76623511769916774, 13.28545270918177934 ) ) ;
#1259 = CARTESIAN_POINT ( 'NONE',  ( 13.36276861424025775, 57.36259551922253053, 1.924898818614698470 ) ) ;
#1260 = CARTESIAN_POINT ( 'NONE',  ( -9.520470885617715595, 68.62999999999999545, -6.917026985038136289 ) ) ;
#1261 = CARTESIAN_POINT ( 'NONE',  ( -8.343458848123582072, 37.37999999999999545, 11.48378591275254124 ) ) ;
#1262 = CARTESIAN_POINT ( 'NONE',  ( -3.636496289402155746, 72.53000000000000114, 11.19198476289190936 ) ) ;
#1263 = CARTESIAN_POINT ( 'NONE',  ( -11.46982637885754563, 47.19613723285193174, 7.120329246312594229 ) ) ;
#1264 = DIRECTION ( 'NONE',  ( 0.000000000000000000, 0.000000000000000000, 1.000000000000000000 ) ) ;
#1265 = CARTESIAN_POINT ( 'NONE',  ( 3.675929408452784486, -99.99999999999997158, 14.71521157600635910 ) ) ;
#1266 = CARTESIAN_POINT ( 'NONE',  ( -5.314818182906294375, 10.00000000000000888, -11.69530585927466326 ) ) ;
#1267 = CARTESIAN_POINT ( 'NONE',  ( 11.37499999999960565, -91.60937499999975842, 4.711679271994918317 ) ) ;
#1268 =( BOUNDED_CURVE ( )  B_SPLINE_CURVE ( 2, ( #11581, #16956, #5937, #11317, #16695, #10178, #14294, #15355, #14038, #3259, #6277, #15703, #8593 ),
 .UNSPECIFIED., .F., .F. ) 
 B_SPLINE_CURVE_WITH_KNOTS ( ( 3, 2, 2, 2, 2, 2, 3 ),
 ( 0.5694444444444444198, 0.5722222222222221877, 0.5777777777777777235, 0.5833333333333333703, 0.5888888888888889062, 0.5944444444444444420, 0.5972222222222222099 ),
 .UNSPECIFIED. ) 
 CURVE ( )  GEOMETRIC_REPRESENTATION_ITEM ( )  RATIONAL_B_SPLINE_CURVE ( ( 0.9755282581475768211, 0.9755282581475768211, 1.000000000000000000, 0.9510565162951535312, 1.000000000000000000, 0.9510565162951535312, 1.000000000000000000, 0.9510565162951535312, 1.000000000000000000, 0.9510565162951535312, 1.000000000000000000, 0.9755282581475768211, 0.9755282581475768211 ) ) 
 REPRESENTATION_ITEM ( '' )  );
#1269 = DIRECTION ( 'NONE',  ( -0.000000000000000000, 1.000000000000000000, -0.000000000000000000 ) ) ;
#1270 = CARTESIAN_POINT ( 'NONE',  ( 12.20205365874035408, 33.64198225340590653, -5.778782258580305253 ) ) ;
#1271 = CARTESIAN_POINT ( 'NONE',  ( -3.691467218196870625, 73.31271651008955814, -12.98552287576125330 ) ) ;
#1272 = ORIENTED_EDGE ( 'NONE', *, *, #2727, .F. ) ;
#1273 = ORIENTED_EDGE ( 'NONE', *, *, #14405, .T. ) ;
#1274 = CARTESIAN_POINT ( 'NONE',  ( 7.272992578804308828, 75.98000000000000398, 10.01041549318726886 ) ) ;
#1275 = VERTEX_POINT ( 'NONE', #10069 ) ;
#1276 = CARTESIAN_POINT ( 'NONE',  ( 11.37499999999999645, -107.1499999999997783, 9.531744055041752924E-13 ) ) ;
#1277 = CARTESIAN_POINT ( 'NONE',  ( -0.1540485588782081749, 44.67444256847909401, 13.49999999998640554 ) ) ;
#1278 = CARTESIAN_POINT ( 'NONE',  ( -19.00000000000001776, 7.773118517290098950, 1.732050807568674466 ) ) ;
#1279 = CARTESIAN_POINT ( 'NONE',  ( -8.343458848123576743, 46.48000000000000398, -11.48378591275254301 ) ) ;
#1280 = CARTESIAN_POINT ( 'NONE',  ( -13.39973178939295373, 70.87272364588611140, -1.642340154095887517 ) ) ;
#1281 = CARTESIAN_POINT ( 'NONE',  ( 13.16986379959833897, -40.61874999999988489, 13.16986379960055409 ) ) ;
#1282 = CARTESIAN_POINT ( 'NONE',  ( -12.75809247443173788, 67.77074377949604411, -4.416153755955929405 ) ) ;
#1283 = CARTESIAN_POINT ( 'NONE',  ( 1.561832610794586740E-12, 3.087500000000011458, -18.62500000000000000 ) ) ;
#1284 = CARTESIAN_POINT ( 'NONE',  ( 13.48422240914645442, 54.45333625655221965, -0.6766818701643474432 ) ) ;
#1285 = CARTESIAN_POINT ( 'NONE',  ( -3.636496289402156190, 16.53000000000001535, 11.19198476289190758 ) ) ;
#1286 = DIRECTION ( 'NONE',  ( 0.000000000000000000, -1.000000000000000000, 0.000000000000000000 ) ) ;
#1287 = CARTESIAN_POINT ( 'NONE',  ( -12.97482353139810130, 64.79664418661724312, -3.729052729424082280 ) ) ;
#1288 = CARTESIAN_POINT ( 'NONE',  ( -12.56949574550154836, 35.10876493811377941, 4.925247007018846546 ) ) ;
#1289 = EDGE_LOOP ( 'NONE', ( #4809, #499, #4215, #3994 ) ) ;
#1290 = DIRECTION ( 'NONE',  ( 0.000000000000000000, -1.000000000000000000, 0.000000000000000000 ) ) ;
#1291 = CIRCLE ( 'NONE', #16234, 9.500000000000021316 ) ;
#1292 = CARTESIAN_POINT ( 'NONE',  ( -10.28350456035710003, 31.59411424244996880, -8.747300393376729488 ) ) ;
#1293 = CARTESIAN_POINT ( 'NONE',  ( 4.040337042483869823, 73.03468595069342939, -12.88447105581200169 ) ) ;
#1294 = CARTESIAN_POINT ( 'NONE',  ( 2.279995255611139653E-15, -8.820000000000000284, -12.37355403259654985 ) ) ;
#1295 = CARTESIAN_POINT ( 'NONE',  ( -11.00000000000012612, 0.000000000000000000, 15.58845726811980725 ) ) ;
#1296 = CARTESIAN_POINT ( 'NONE',  ( 2.621994543952811015E-15, -3.820000000000004281, -14.19474002721660355 ) ) ;
#1297 = CARTESIAN_POINT ( 'NONE',  ( -9.907842913857002998, 53.28558844465230493, 9.169773063847259209 ) ) ;
#1298 = ADVANCED_FACE ( 'NONE', ( #12702 ), #4575, .F. ) ;
#1299 = CARTESIAN_POINT ( 'NONE',  ( -7.272992578804307939, 47.47999999999998977, -10.01041549318726886 ) ) ;
#1300 = CARTESIAN_POINT ( 'NONE',  ( 13.50000000000000000, 68.43000000000000682, 1.653273178848926867E-15 ) ) ;
#1301 = CARTESIAN_POINT ( 'NONE',  ( 4.977012011971282845, 50.85955796876759649, 12.54907956735184982 ) ) ;
#1302 = AXIS2_PLACEMENT_3D ( 'NONE', #3178, #5860, #10015 ) ;
#1303 = CARTESIAN_POINT ( 'NONE',  ( -7.545992825712033003, 37.46287733677418430, -11.19724308666464019 ) ) ;
#1304 = CARTESIAN_POINT ( 'NONE',  ( 13.37272337869130823, 36.36494487923371821, 1.858079212359092569 ) ) ;
#1305 = CARTESIAN_POINT ( 'NONE',  ( 4.711679271993006957, -87.37812499999982663, 11.37500000000039257 ) ) ;
#1306 = CARTESIAN_POINT ( 'NONE',  ( -11.21338182703946451, 74.21242793460713472, 7.517659778229184298 ) ) ;
#1307 = CARTESIAN_POINT ( 'NONE',  ( -12.52141048085782948, 76.74656338183874027, -5.046232787786422591 ) ) ;
#1308 = CARTESIAN_POINT ( 'NONE',  ( -13.15667449852409021, 80.03835353115930218, 3.056836537833763856 ) ) ;
#1309 = CARTESIAN_POINT ( 'NONE',  ( 7.500000000000000000, 106.5806336763438793, -7.726132535793191813 ) ) ;
#1310 = DIRECTION ( 'NONE',  ( -1.000000000000000000, -0.000000000000000000, -0.000000000000000000 ) ) ;
#1311 = CARTESIAN_POINT ( 'NONE',  ( 2.279995255611139653E-15, 0.1800000000000001044, -12.37355403259654985 ) ) ;
#1312 = CARTESIAN_POINT ( 'NONE',  ( 9.520470885617717371, 49.72999999999999687, -6.917026985038131848 ) ) ;
#1313 = CARTESIAN_POINT ( 'NONE',  ( 4.711679271993006068, -13.52812499999996732, 11.37500000000039257 ) ) ;
#1314 = CARTESIAN_POINT ( 'NONE',  ( -1.564113515457998572E-12, -45.78749999999988773, 18.62500000000000000 ) ) ;
#1315 = CARTESIAN_POINT ( 'NONE',  ( 13.50000000000000000, -5.569999999999998508, 1.734723475976807094E-15 ) ) ;
#1316 = CARTESIAN_POINT ( 'NONE',  ( 10.92172942406178926, 35.13000000000000256, 7.935100905948387684 ) ) ;
#1317 = CARTESIAN_POINT ( 'NONE',  ( 10.95438131901840961, 75.72796546381928806, -7.891384625383862428 ) ) ;
#1318 = CYLINDRICAL_SURFACE ( 'NONE', #16121, 26.00000000000000355 ) ;
#1319 = CARTESIAN_POINT ( 'NONE',  ( -7.272992578804310604, 42.37999999999999545, 10.01041549318726709 ) ) ;
#1320 = CARTESIAN_POINT ( 'NONE',  ( -9.383695827828427483, 41.31213889170596332, 9.705529900550189382 ) ) ;
#1321 = CARTESIAN_POINT ( 'NONE',  ( -5.764561566141782833, 58.38968915241470370, -12.20736831470176398 ) ) ;
#1322 = CARTESIAN_POINT ( 'NONE',  ( -12.00000000000000178, 9.895771319534587107, 2.592753011680899000 ) ) ;
#1323 = CARTESIAN_POINT ( 'NONE',  ( -13.49999999999999822, 55.08000000000000540, 4.386415899144235020 ) ) ;
#1324 = CYLINDRICAL_SURFACE ( 'NONE', #9888, 5.000000000000000000 ) ;
#1325 = CARTESIAN_POINT ( 'NONE',  ( -10.10360367143677429, 55.58467546146358274, -8.953613654375507380 ) ) ;
#1326 = CARTESIAN_POINT ( 'NONE',  ( -10.78023278508444349, 49.62152785118134801, -8.131429254652333682 ) ) ;
#1327 = CARTESIAN_POINT ( 'NONE',  ( 11.45531800585675519, 63.69692067607217467, -7.143501120740932464 ) ) ;
#1328 = CARTESIAN_POINT ( 'NONE',  ( 12.00345388897867061, 42.65789368871043763, -6.178225835024248269 ) ) ;
#1329 = CARTESIAN_POINT ( 'NONE',  ( -18.11515225121977579, 8.027996313748971602, -0.6918446750616502605 ) ) ;
#1330 = ORIENTED_EDGE ( 'NONE', *, *, #4889, .T. ) ;
#1331 = CARTESIAN_POINT ( 'NONE',  ( -8.121902954028387356, 70.48834023284237560, -10.78388806788330534 ) ) ;
#1332 = CARTESIAN_POINT ( 'NONE',  ( 11.37500000000039435, -1.040624999999997025, -4.711679271993003404 ) ) ;
#1333 = ORIENTED_EDGE ( 'NONE', *, *, #12837, .T. ) ;
#1334 = ORIENTED_EDGE ( 'NONE', *, *, #1418, .F. ) ;
#1335 = CARTESIAN_POINT ( 'NONE',  ( 13.50000000000000000, 18.43000000000000327, 1.734723475976807094E-15 ) ) ;
#1336 = CARTESIAN_POINT ( 'NONE',  ( 13.16986379959834075, -47.86874999999988489, 13.16986379960055231 ) ) ;
#1337 = CARTESIAN_POINT ( 'NONE',  ( 11.49604287478703135, 60.69423318969604964, -7.077870380912349546 ) ) ;
#1338 = CARTESIAN_POINT ( 'NONE',  ( -13.50000000000000000, 14.92999999999999972, -3.469446951953614189E-15 ) ) ;
#1339 = CARTESIAN_POINT ( 'NONE',  ( 7.579234238537092772, 71.96436601207575734, 11.17165930700318910 ) ) ;
#1340 = CARTESIAN_POINT ( 'NONE',  ( 12.81014742043414678, 57.58654023661487997, -4.352113031915539665 ) ) ;
#1341 = ADVANCED_FACE ( 'NONE', ( #8997 ), #4231, .T. ) ;
#1342 = CARTESIAN_POINT ( 'NONE',  ( -9.520470885617717371, 72.23000000000000398, 6.917026985038133624 ) ) ;
#1343 = CARTESIAN_POINT ( 'NONE',  ( 3.636496289402157078, 77.03000000000000114, -11.19198476289190936 ) ) ;
#1344 = ADVANCED_FACE ( 'NONE', ( #11290 ), #14355, .F. ) ;
#1345 = CARTESIAN_POINT ( 'NONE',  ( -10.34620229525405577, 47.26236668688625997, 8.674891611129472935 ) ) ;
#1346 = CARTESIAN_POINT ( 'NONE',  ( -12.50000000000000000, 102.9300000000000210, 1.714505518806294638E-15 ) ) ;
#1347 = CARTESIAN_POINT ( 'NONE',  ( 7.416407864998777910, 9.013974596215598822, -10.20780970022453182 ) ) ;
#1348 = CARTESIAN_POINT ( 'NONE',  ( 5.439017319324713107, -99.99999999999994316, 15.41596283236346032 ) ) ;
#1349 = CARTESIAN_POINT ( 'NONE',  ( 0.000000000000000000, 30.93000000000001393, 0.000000000000000000 ) ) ;
#1350 = CARTESIAN_POINT ( 'NONE',  ( 4.711679271993006068, -13.52812499999996732, 11.37500000000039257 ) ) ;
#1351 = CARTESIAN_POINT ( 'NONE',  ( -8.291044507619272909E-14, 7.180000000000005045, -13.50000000000000000 ) ) ;
#1352 = CARTESIAN_POINT ( 'NONE',  ( 13.48916840549102325, 33.44861295401204160, -0.5407753439385338812 ) ) ;
#1353 = CARTESIAN_POINT ( 'NONE',  ( -9.418482302422065189, 73.54949279931506112, -9.674530453309715838 ) ) ;
#1354 = ORIENTED_EDGE ( 'NONE', *, *, #5085, .T. ) ;
#1355 = EDGE_LOOP ( 'NONE', ( #1938, #7619, #9625, #947 ) ) ;
#1356 = CARTESIAN_POINT ( 'NONE',  ( -10.92172942406178926, 42.63000000000000256, -7.935100905948389460 ) ) ;
#1357 = ORIENTED_EDGE ( 'NONE', *, *, #595, .F. ) ;
#1358 = CARTESIAN_POINT ( 'NONE',  ( -13.32969872981109738, 41.00498912793175066, 2.137555216804883695 ) ) ;
#1359 = CARTESIAN_POINT ( 'NONE',  ( 9.538709233711902776E-13, -78.01249999999981810, -11.37499999999999645 ) ) ;
#1360 = CARTESIAN_POINT ( 'NONE',  ( -0.6995756356649440733, 44.65484589472355736, 13.48186430673500347 ) ) ;
#1361 = CARTESIAN_POINT ( 'NONE',  ( -7.499999999999997335, -24.46203974633109368, 8.709571264514707423 ) ) ;
#1362 = AXIS2_PLACEMENT_3D ( 'NONE', #12059, #5527, #1264 ) ;
#1363 = CARTESIAN_POINT ( 'NONE',  ( 13.49999999999999822, 45.28000000000000114, 4.386415899144237684 ) ) ;
#1364 = CARTESIAN_POINT ( 'NONE',  ( 2.607531440858944223E-15, 45.17999999999999972, -14.19474002721660355 ) ) ;
#1365 = CARTESIAN_POINT ( 'NONE',  ( -13.41563146330035572, 70.87746431999256913, -1.508872100732321142 ) ) ;
#1366 = ADVANCED_FACE ( 'NONE', ( #1900 ), #14271, .T. ) ;
#1367 =( BOUNDED_CURVE ( )  B_SPLINE_CURVE ( 2, ( #15529, #8936, #10347, #6194, #11665, #2180, #7606, #7255, #3438, #4601, #527, #3352, #12984 ),
 .UNSPECIFIED., .F., .F. ) 
 B_SPLINE_CURVE_WITH_KNOTS ( ( 3, 2, 2, 2, 2, 2, 3 ),
 ( 0.4027777777777777901, 0.4055555555555555580, 0.4111111111111110938, 0.4166666666666666852, 0.4222222222222222210, 0.4277777777777777568, 0.4305555555555555247 ),
 .UNSPECIFIED. ) 
 CURVE ( )  GEOMETRIC_REPRESENTATION_ITEM ( )  RATIONAL_B_SPLINE_CURVE ( ( 0.9755282581475768211, 0.9755282581475768211, 1.000000000000000000, 0.9510565162951535312, 1.000000000000000000, 0.9510565162951535312, 1.000000000000000000, 0.9510565162951535312, 1.000000000000000000, 0.9510565162951535312, 1.000000000000000000, 0.9755282581475770431, 0.9755282581475768211 ) ) 
 REPRESENTATION_ITEM ( '' )  );
#1368 = CARTESIAN_POINT ( 'NONE',  ( 1.561832610794586740E-12, -30.21249999999990976, -18.62500000000000000 ) ) ;
#1369 = CARTESIAN_POINT ( 'NONE',  ( -12.00546221442099082, 67.70198623451226183, -6.182780363064463103 ) ) ;
#1370 = CARTESIAN_POINT ( 'NONE',  ( -1.564113515457998370E-12, -21.88749999999992824, 18.62500000000000000 ) ) ;
#1371 = CARTESIAN_POINT ( 'NONE',  ( 13.50008151215212671, 54.43042949225134208, -0.01282350395396137689 ) ) ;
#1372 = PRESENTATION_LAYER_ASSIGNMENT (  '', '', ( #4497 ) ) ;
#1373 = CARTESIAN_POINT ( 'NONE',  ( -18.62500000000064659, -75.96562499999980389, 7.714727599197335195 ) ) ;
#1374 = CARTESIAN_POINT ( 'NONE',  ( -12.01698627149207255, 64.70299437077932225, -6.156538469565180804 ) ) ;
#1375 = CARTESIAN_POINT ( 'NONE',  ( -13.50000000000000000, 63.92999999999999972, -3.306546357697853733E-15 ) ) ;
#1376 = CARTESIAN_POINT ( 'NONE',  ( -13.47844695735242126, 34.96030382913254897, 0.8794953320084257786 ) ) ;
#1377 = VERTEX_POINT ( 'NONE', #16754 ) ;
#1378 = CARTESIAN_POINT ( 'NONE',  ( -10.16733827920521804, 1.259542957514475215E-16, -7.849773118324066878 ) ) ;
#1379 = CARTESIAN_POINT ( 'NONE',  ( -0.2969749873785103578, 31.19067812498207104, -13.50000000000000711 ) ) ;
#1380 = CARTESIAN_POINT ( 'NONE',  ( 5.463127872796244233, 72.98208016960933264, -12.34858486968830427 ) ) ;
#1381 = CARTESIAN_POINT ( 'NONE',  ( 11.76794919243112680, -12.42000000000000171, -3.823638476888993942 ) ) ;
#1382 = CYLINDRICAL_SURFACE ( 'NONE', #8332, 9.000000000000000000 ) ;
#1383 = CARTESIAN_POINT ( 'NONE',  ( -8.343458848123582072, -11.62000000000000632, 11.48378591275254124 ) ) ;
#1384 = CARTESIAN_POINT ( 'NONE',  ( -13.46935105989159354, 52.89853437352409316, -0.9121747106428150786 ) ) ;
#1385 = EDGE_CURVE ( 'NONE', #4199, #17188, #4662, .T. ) ;
#1386 = AXIS2_PLACEMENT_3D ( 'NONE', #9999, #15171, #10961 ) ;
#1387 = CARTESIAN_POINT ( 'NONE',  ( -7.272992578804307939, 50.47999999999999687, -10.01041549318726886 ) ) ;
#1388 = CARTESIAN_POINT ( 'NONE',  ( -8.343458848123582072, 64.37999999999998124, 11.48378591275254124 ) ) ;
#1389 = CARTESIAN_POINT ( 'NONE',  ( 4.440954443873683211, 50.83963344985475885, 12.75191637729435357 ) ) ;
#1390 = CARTESIAN_POINT ( 'NONE',  ( -5.576691037129440254, 37.38238622676195888, -12.29433165838705300 ) ) ;
#1391 = CARTESIAN_POINT ( 'NONE',  ( 4.653539263734507436, 35.84745211565388701, 12.67597189436627403 ) ) ;
#1392 = CARTESIAN_POINT ( 'NONE',  ( 18.62500000000064659, -24.94062499999996518, -7.714727599197336083 ) ) ;
#1393 = CARTESIAN_POINT ( 'NONE',  ( -11.25831317180859692, 74.20964794744398318, 7.449907306601299517 ) ) ;
#1394 = CARTESIAN_POINT ( 'NONE',  ( -10.39579503320424436, 76.60004714428708894, -8.615611839668220640 ) ) ;
#1395 = CARTESIAN_POINT ( 'NONE',  ( -9.858077159528473743, 79.57156653839524552, -9.233591285681558958 ) ) ;
#1396 = CARTESIAN_POINT ( 'NONE',  ( -7.272992578804307939, 9.480000000000009308, -10.01041549318726886 ) ) ;
#1397 = CARTESIAN_POINT ( 'NONE',  ( 4.992525441480580639, 80.92999999999996419, 12.45192268195276952 ) ) ;
#1398 = DIRECTION ( 'NONE',  ( -0.000000000000000000, -1.000000000000000000, -0.000000000000000000 ) ) ;
#1399 = CARTESIAN_POINT ( 'NONE',  ( -11.76794919243112325, 3.780000000000002913, -3.823638476888998827 ) ) ;
#1400 = CARTESIAN_POINT ( 'NONE',  ( -3.636496289402153081, 44.32999999999999829, -11.19198476289190936 ) ) ;
#1401 = CARTESIAN_POINT ( 'NONE',  ( 11.37500000000039435, -50.99062499999987352, -4.711679271993004292 ) ) ;
#1402 = CARTESIAN_POINT ( 'NONE',  ( -13.16986379960055231, -27.05624999999993463, 13.16986379959834252 ) ) ;
#1403 = CARTESIAN_POINT ( 'NONE',  ( -10.92172942406179104, -6.769999999999997797, 7.935100905948385908 ) ) ;
#1404 = CARTESIAN_POINT ( 'NONE',  ( -5.683316182202581501, 40.38652174635834058, -12.24545745996583257 ) ) ;
#1405 = CARTESIAN_POINT ( 'NONE',  ( 0.000000000000000000, 3.000000000000000000, 0.000000000000000000 ) ) ;
#1406 = CARTESIAN_POINT ( 'NONE',  ( 10.26510932771960505, 75.09330710058536340, 8.767992633449631867 ) ) ;
#1407 = CARTESIAN_POINT ( 'NONE',  ( 6.278630761140489902, 1.381986750647006550E-15, -11.02614667217763511 ) ) ;
#1408 = CARTESIAN_POINT ( 'NONE',  ( -3.636496289402153081, 44.32999999999999829, -11.19198476289190936 ) ) ;
#1409 = CARTESIAN_POINT ( 'NONE',  ( -11.68127071909253090, 41.18172457130780373, 6.770866295227015996 ) ) ;
#1410 = CARTESIAN_POINT ( 'NONE',  ( -8.422466027777701925, 58.50203747567191215, -10.55087072492730726 ) ) ;
#1411 = CARTESIAN_POINT ( 'NONE',  ( -8.891200544363830713E-16, 58.67999999999999261, 13.50000000000000000 ) ) ;
#1412 = CARTESIAN_POINT ( 'NONE',  ( 6.750022862106053623, 29.92926176209967437, 11.69132975161703669 ) ) ;
#1413 = CARTESIAN_POINT ( 'NONE',  ( -19.00000000000001776, 0.000000000000000000, 1.732050807568674466 ) ) ;
#1414 = CARTESIAN_POINT ( 'NONE',  ( -13.47356114761061896, 49.90085270701082720, -0.8452802774780980855 ) ) ;
#1415 = CARTESIAN_POINT ( 'NONE',  ( 13.36701738278523699, 63.49611584409814213, -1.890200968080443911 ) ) ;
#1416 = CARTESIAN_POINT ( 'NONE',  ( 12.32211066819836986, 42.22827443285392235, 5.515240709522629459 ) ) ;
#1417 = CARTESIAN_POINT ( 'NONE',  ( 1.448380041428809273, 38.73207828558371801, 13.42211311086453485 ) ) ;
#1418 = EDGE_CURVE ( 'NONE', #7389, #9499, #14638, .T. ) ;
#1419 = VERTEX_POINT ( 'NONE', #2071 ) ;
#1420 = PLANE ( 'NONE',  #7136 ) ;
#1421 = LINE ( 'NONE', #2827, #9613 ) ;
#1422 = CARTESIAN_POINT ( 'NONE',  ( -4.171729424061787483, 16.33000000000001251, -12.83926296998457417 ) ) ;
#1423 = ORIENTED_EDGE ( 'NONE', *, *, #12269, .F. ) ;
#1424 = CARTESIAN_POINT ( 'NONE',  ( -5.008917595718572535, 43.36076862181904801, -12.53804254533077689 ) ) ;
#1425 = CARTESIAN_POINT ( 'NONE',  ( -7.499999999999998224, 108.4757119436330584, 3.584587286925195126 ) ) ;
#1426 = CARTESIAN_POINT ( 'NONE',  ( 9.798639380625722595, 60.79125297211457735, -9.294035878196183376 ) ) ;
#1427 = CARTESIAN_POINT ( 'NONE',  ( 13.50000000000000000, 10.42999999999999439, 1.734723475976807094E-15 ) ) ;
#1428 = CARTESIAN_POINT ( 'NONE',  ( -1.900613283894436512, 7.469143981464171134, 12.00000000000000000 ) ) ;
#1429 = CARTESIAN_POINT ( 'NONE',  ( 12.77134458573675602, 66.58771978361312449, -4.375411503001064517 ) ) ;
#1430 = CARTESIAN_POINT ( 'NONE',  ( 3.922183893232446650, 56.82075162799759482, 12.92321760331618030 ) ) ;
#1431 = CARTESIAN_POINT ( 'NONE',  ( -11.76794919243112325, 68.77999999999998693, -3.823638476888998827 ) ) ;
#1432 = CARTESIAN_POINT ( 'NONE',  ( 11.76794919243112680, 64.57999999999999829, -3.823638476888993942 ) ) ;
#1433 = CARTESIAN_POINT ( 'NONE',  ( -7.335511309088512455, 47.40615135898282517, 11.33352093287819073 ) ) ;
#1434 = DIRECTION ( 'NONE',  ( 0.000000000000000000, -1.000000000000000000, 0.000000000000000000 ) ) ;
#1435 = CARTESIAN_POINT ( 'NONE',  ( 9.708203932499419153, 8.263974596215597046, 7.053423027509715837 ) ) ;
#1436 = CARTESIAN_POINT ( 'NONE',  ( 18.55057311700109324, -99.99999999999998579, 1.729945603080623062 ) ) ;
#1437 = CARTESIAN_POINT ( 'NONE',  ( -2.198133652130575211, 56.60094066944324709, 13.31991233539677921 ) ) ;
#1438 = CARTESIAN_POINT ( 'NONE',  ( 11.37499999999960210, -48.90937499999989058, 4.711679271994918317 ) ) ;
#1439 = DIRECTION ( 'NONE',  ( 0.000000000000000000, -1.000000000000000000, 0.000000000000000000 ) ) ;
#1440 = CARTESIAN_POINT ( 'NONE',  ( 12.00158882157005991, 33.65803713169809441, -6.181575385805966327 ) ) ;
#1441 = CARTESIAN_POINT ( 'NONE',  ( -9.967793045472657099, 73.57753319009304960, -9.105432612504264611 ) ) ;
#1442 = CARTESIAN_POINT ( 'NONE',  ( -7.999999999999777955, 7.836096772789082010, -17.06161034813192146 ) ) ;
#1443 = CARTESIAN_POINT ( 'NONE',  ( -9.520470885617717371, 25.23000000000000398, 6.917026985038133624 ) ) ;
#1444 = ADVANCED_FACE ( 'NONE', ( #7582 ), #6173, .T. ) ;
#1445 = ORIENTED_EDGE ( 'NONE', *, *, #3312, .T. ) ;
#1446 = CARTESIAN_POINT ( 'NONE',  ( -5.032544374794751363, 62.49832613186128327, 12.52840728639462853 ) ) ;
#1447 = ORIENTED_EDGE ( 'NONE', *, *, #6481, .T. ) ;
#1448 = APPLICATION_CONTEXT ( 'automotive_design' ) ;
#1449 = CARTESIAN_POINT ( 'NONE',  ( -4.711679271993001628, -79.05312499999985221, -11.37500000000039613 ) ) ;
#1450 = CARTESIAN_POINT ( 'NONE',  ( -13.18851637220922690, 44.03230396172555317, 2.886947055359128100 ) ) ;
#1451 = VECTOR ( 'NONE', #8697, 1000.000000000000000 ) ;
#1452 = CARTESIAN_POINT ( 'NONE',  ( -7.499999999999995559, -27.79702113870391145, 1.010069558262734590 ) ) ;
#1453 = CARTESIAN_POINT ( 'NONE',  ( 10.92172942406179104, 45.72999999999999687, -7.935100905948385908 ) ) ;
#1454 = CARTESIAN_POINT ( 'NONE',  ( 8.343458848123578520, 49.97999999999998977, 11.48378591275254124 ) ) ;
#1455 = CARTESIAN_POINT ( 'NONE',  ( -13.49749511909229938, 70.92107257862903680, -0.2602492951671970256 ) ) ;
#1456 = CARTESIAN_POINT ( 'NONE',  ( 13.16986379960055409, -11.48124999999995488, -13.16986379959834430 ) ) ;
#1457 = CARTESIAN_POINT ( 'NONE',  ( -2.939452924911615028, 67.28569332682523907, -13.17610025439934418 ) ) ;
#1458 = CARTESIAN_POINT ( 'NONE',  ( 18.62500000000064659, -10.44062499999995453, -7.714727599197336083 ) ) ;
#1459 = CIRCLE ( 'NONE', #14167, 1.999999999999998224 ) ;
#1460 = CARTESIAN_POINT ( 'NONE',  ( 13.42620872007250021, 54.48099588213615618, -1.465427023774013238 ) ) ;
#1461 = CARTESIAN_POINT ( 'NONE',  ( -13.12121150380120405, 65.04454592078904795, 3.225014459927483479 ) ) ;
#1462 = EDGE_CURVE ( 'NONE', #15411, #6381, #10321, .T. ) ;
#1463 = ORIENTED_EDGE ( 'NONE', *, *, #1049, .T. ) ;
#1464 = CARTESIAN_POINT ( 'NONE',  ( -2.138189944381236884, 63.25688142232026223, -13.50000000000000000 ) ) ;
#1465 = CARTESIAN_POINT ( 'NONE',  ( -13.01212560558737685, 34.80158386758054689, -3.596716132205523220 ) ) ;
#1466 = EDGE_LOOP ( 'NONE', ( #9715, #8478, #9152, #5189 ) ) ;
#1467 = CARTESIAN_POINT ( 'NONE',  ( 12.85971963305189902, 78.28239814670027386, 4.108247630965401243 ) ) ;
#1468 = CARTESIAN_POINT ( 'NONE',  ( 1.653273178848926472E-15, 80.93000000000000682, 13.50000000000000000 ) ) ;
#1469 = CARTESIAN_POINT ( 'NONE',  ( -3.039705960452427469, 31.28929609180920579, -13.15420631222019132 ) ) ;
#1470 = CARTESIAN_POINT ( 'NONE',  ( 10.29308383338549859, 72.76519627777207688, -8.735152889481485161 ) ) ;
#1471 = CARTESIAN_POINT ( 'NONE',  ( -11.76794919243112325, -8.070000000000000284, -2.602085213965210642E-15 ) ) ;
#1472 = CARTESIAN_POINT ( 'NONE',  ( 5.441113646577305119, 0.000000000000000000, 25.42428528562857792 ) ) ;
#1473 = CARTESIAN_POINT ( 'NONE',  ( -8.343458848123576743, -15.52000000000000668, -11.48378591275254301 ) ) ;
#1474 =( BOUNDED_SURFACE ( )  B_SPLINE_SURFACE ( 1, 2, ( 
 ( #12835, #2432, #5956, #8696, #15373, #12918, #10109, #3279, #12745, #14056, #6043, #15461, #14142, #2030, #3540, #801, #10280, #4793, #722, #6131, #10194, #11598, #14227, #11511, #16886, #15547, #8873, #3459, #14547, #7538, #6212, #7864, #16975, #4877, #15631, #462, #5209, #10599, #11918, #2520, #17296, #9282, #15962, #13238, #14634, #3867, #1126, #6538, #8519, #40, #12650, #15100, #16707, #9846, #1853, #11243, #15281, #8429, #16194, #16622, #8780, #12481, #5445, #5864, #5949, #11329, #3093, #5772, #16532, #3182, #10832, #4106, #627, #1681, #13956, #7097, #9755, #12568, #4439, #2999, #15367, #14136, #2024, #15193, #4612, #13783, #367, #11156, #1937, #4699, #13869, #1771, #7180, #9932, #8690, #10019, #454, #6038, #16793, #7266, #10104, #4525, #8604, #15455, #12152, #3365, #12739, #540, #3273, #14049, #7360, #11421, #11678, #4787, #15895, #12912, #2105, #4871, #6469, #10274, #6206, #17054, #15541, #8948, #796, #6291, #3803, #6126, #14390, #3453, #11505, #879, #12997, #7449, #17141, #968, #4959, #7706, #7532, #10362, #16881, #2193, #13082, #14567, #10187, #7800, #8868, #11592, #14220, #10448, #13171, #16968, #715, #15625, #9037, #2366, #3533, #14306, #7621, #15716, #3620, #2279, #6382, #11765, #5050, #15807, #3711, #9129, #14478, #5140, #1057, #11855, #17230, #10532, #9215, #12828, #11936, #17317, #3974, #2451, #2541, #2625, #4241, #14653, #9473, #8236, #9650, #5230, #13507, #1492, #17401, #9561, #5490, #3885, #17485, #1229, #10615, #12022, #12192, #178, #13422, #1399, #7969, #7881, #8058, #16150, #13258, #1145, #4058, #15982, #9302, #6556, #10871, #9386, #13338, #6641, #5316, #6815, #10700, #16240, #16068, #4149, #14737, #16333, #13596, #1311, #6726, #14821, #12104, #85, #5400, #10784, #14911, #10965, #2715, #8144, #2804, #6907, #5584, #12283, #16775, #6996, #5845, #16425, #9737, #265, #16688, #8413, #2893, #1665, #610, #10002, #7340, #1833, #15263, #9915, #7250, #8675, #11311, #2982, #9830, #15083, #5931, #7165, #6019, #4595, #16514, #4683, #3251, #3075, #523, #4329, #8501, #12551, #7080, #11402, #12464, #15349, #13851, #15000, #12634, #13939, #8325, #13764, #11139, #13680, #3161, #5673, #14032, #348, #4509, #1754, #437, #11053, #1578, #11228, #12371, #5755, #4421, #16602, #8588, #1920, #15175, #12723, #2499, #16028, #6431, #11815, #44, #11985, #16198, #7758, #6867, #2944, #12332, #5541, #16565, #9961, #8195, #16385, #1715, #135, #10925, #4201, #15226, #486, #4289, #9700, #8373, #16473, #4471, #398, #13729, #13901, #13558, #15134, #7045, #12424, #4379, #3031, #8462, #12514, #3123, #746, #14248, #12767, #11361, #13986, #2053, #12682, #6320, #3305, #10048, #656, #14333, #6065, #14078 ),
 ( #12856, #15398, #2134, #5979, #11620, #13027, #4901, #14164, #7651, #3214, #572, #10215, #8635, #7560, #1881, #16822, #6233, #11706, #8718, #7476, #16995, #1965, #909, #2222, #17083, #7297, #6155, #16736, #7390, #4642, #10300, #4729, #10130, #11532, #15483, #3394, #8807, #16910, #4988, #4813, #15568, #3479, #8893, #12938, #822, #15311, #15653, #3563, #8977, #10643, #10477, #9245, #9067, #5170, #16007, #20, #14420, #10726, #2308, #15837, #7736, #13365, #16091, #13112, #3655, #999, #11966, #5341, #6412, #3742, #11795, #15922, #13286, #3830, #17172, #5082, #7911, #9158, #9330, #14505, #6665, #8084, #17426, #14598, #2655, #13449, #2393, #13200, #1086, #6500, #11883, #10390, #17258, #10562, #12131, #2478, #17346, #3999, #15744, #1174, #3913, #9415, #6585, #14763, #1254, #5257, #14680, #2567, #7997, #12049, #1335, #6751, #9176, #14846, #9087, #5605, #3764, #11900, #8993, #14350, #5190, #13046, #928, #15672, #1422, #10494, #2239, #6338, #17100, #2739, #10406, #6839, #15763, #12215, #14440, #12306, #9586, #109, #7757, #6928, #14936, #13132, #1020, #6520, #6430, #11814, #17191, #5514, #15857, #14524, #2411, #10810, #4083, #9498, #8169, #13532, #10897, #16267, #4173, #2828, #8259, #16537, #10987, #3187, #4530, #8524, #11248, #11075, #9851, #9673, #5777, #16627, #4263, #2916, #11334, #8346, #16448, #13702, #13961, #16712, #1602, #7018, #12396, #12573, #5954, #4351, #9760, #15105, #4444, #13874, #15198, #3004, #8434, #1776, #13788, #9937, #1686, #545, #8695, #4617, #3098, #3278, #14055, #7102, #12486, #372, #11162, #460, #5869, #8609, #10024, #12744, #15372, #1942, #17146, #7805, #14141, #17059, #5055, #3458, #13089, #9042, #7454, #3538, #4792, #2029, #15546, #3625, #3716, #16974, #10367, #11510, #13176, #11597, #2198, #4704, #15460, #885, #3371, #12834, #10193, #7711, #12917, #14226, #2110, #6211, #10453, #4876, #15812, #10279, #9134, #15630, #8953, #14483, #14311, #6297, #11683, #6474, #5404, #11860, #15985, #9478, #9564, #1150, #17405, #6645, #1062, #10788, #12108, #16072, #1315, #6561, #5320, #17235, #13342, #6730, #8239, #5145, #1403, #10537, #11942, #15899, #4063, #6819, #3808, #9221, #14572, #2630, #13511, #2456, #17322, #7886, #12026, #3978, #10704, #13263, #5234, #9390, #10619, #3115, #3889, #14825, #16245, #8148, #14741, #10875, #4152, #9306, #14657, #2545, #7973, #1233, #8062, #13426, #16154, #2808, #2719, #12196, #89, #5494, #14914, #7167, #12637, #11055, #3163, #16605, #15002, #11141, #12374, #16335, #5675, #5847, #11313, #7082, #12553, #1580, #3255, #1668, #9832, #1495, #12285, #15177, #5587, #10967, #13599, #9917, #2984, #6909, #4243, #15352, #439, #180, #15267, #9652, #8590, #2895, #10005 ) ),
 .UNSPECIFIED., .F., .F., .F. ) 
 B_SPLINE_SURFACE_WITH_KNOTS ( ( 2, 2 ),
 ( 3, 2, 2, 2, 2, 2, 2, 2, 2, 2, 2, 2, 2, 2, 2, 2, 2, 2, 2, 2, 2, 2, 2, 2, 2, 2, 2, 2, 2, 2, 2, 2, 2, 2, 2, 2, 2, 2, 2, 2, 2, 2, 2, 2, 2, 2, 2, 2, 2, 2, 2, 2, 2, 2, 2, 2, 2, 2, 2, 2, 2, 2, 2, 2, 2, 2, 2, 2, 2, 2, 2, 2, 2, 2, 2, 2, 2, 2, 2, 2, 2, 2, 2, 2, 2, 2, 2, 2, 2, 2, 2, 2, 2, 2, 2, 2, 2, 2, 2, 2, 2, 2, 2, 2, 2, 2, 2, 2, 2, 2, 2, 2, 2, 2, 2, 2, 2, 2, 2, 2, 2, 2, 2, 2, 2, 2, 2, 2, 2, 2, 2, 2, 2, 2, 2, 2, 2, 2, 2, 2, 2, 2, 2, 2, 2, 2, 2, 2, 2, 2, 2, 2, 2, 2, 2, 2, 2, 2, 2, 2, 2, 2, 2, 2, 2, 2, 2, 2, 2, 2, 2, 2, 2, 2, 2, 2, 2, 2, 3 ),
 ( 0.000000000000000000, 1.000000000000000000 ),
 ( 0.000000000000000000, 0.005555555555555555768, 0.01111111111111111154, 0.01666666666666666644, 0.02222222222222222307, 0.02777777777777777624, 0.03333333333333333287, 0.03888888888888888951, 0.04444444444444444614, 0.05000000000000000278, 0.05555555555555555247, 0.06111111111111110911, 0.06666666666666666574, 0.07222222222222221544, 0.07777777777777777901, 0.08333333333333332871, 0.08888888888888889228, 0.09444444444444444198, 0.1000000000000000056, 0.1055555555555555552, 0.1111111111111111049, 0.1166666666666666685, 0.1222222222222222182, 0.1277777777777777679, 0.1333333333333333315, 0.1388888888888888951, 0.1444444444444444309, 0.1499999999999999944, 0.1555555555555555580, 0.1611111111111111216, 0.1666666666666666574, 0.1722222222222222210, 0.1777777777777777846, 0.1833333333333333204, 0.1888888888888888840, 0.1944444444444444475, 0.2000000000000000111, 0.2055555555555555469, 0.2111111111111111105, 0.2166666666666666741, 0.2222222222222222099, 0.2277777777777777735, 0.2333333333333333370, 0.2388888888888889006, 0.2444444444444444364, 0.2500000000000000000, 0.2555555555555555358, 0.2611111111111111271, 0.2666666666666666630, 0.2722222222222221988, 0.2777777777777777901, 0.2833333333333333259, 0.2888888888888888618, 0.2944444444444444531, 0.2999999999999999889, 0.3055555555555555802, 0.3111111111111111160, 0.3166666666666666519, 0.3222222222222222432, 0.3277777777777777790, 0.3333333333333333148, 0.3388888888888889062, 0.3444444444444444420, 0.3499999999999999778, 0.3555555555555555691, 0.3611111111111111049, 0.3666666666666666408, 0.3722222222222222321, 0.3777777777777777679, 0.3833333333333333592, 0.3888888888888888951, 0.3944444444444444309, 0.4000000000000000222, 0.4055555555555555580, 0.4111111111111110938, 0.4166666666666666852, 0.4222222222222222210, 0.4277777777777777568, 0.4333333333333333481, 0.4388888888888888840, 0.4444444444444444198, 0.4500000000000000111, 0.4555555555555555469, 0.4611111111111111382, 0.4666666666666666741, 0.4722222222222222099, 0.4777777777777778012, 0.4833333333333333370, 0.4888888888888888729, 0.4944444444444444642, 0.5000000000000000000, 0.5055555555555555358, 0.5111111111111110716, 0.5166666666666667185, 0.5222222222222222543, 0.5277777777777777901, 0.5333333333333333259, 0.5388888888888888618, 0.5444444444444443976, 0.5500000000000000444, 0.5555555555555555802, 0.5611111111111111160, 0.5666666666666666519, 0.5722222222222221877, 0.5777777777777777235, 0.5833333333333333703, 0.5888888888888889062, 0.5944444444444444420, 0.5999999999999999778, 0.6055555555555555136, 0.6111111111111111605, 0.6166666666666666963, 0.6222222222222222321, 0.6277777777777777679, 0.6333333333333333037, 0.6388888888888888395, 0.6444444444444444864, 0.6500000000000000222, 0.6555555555555555580, 0.6611111111111110938, 0.6666666666666666297, 0.6722222222222222765, 0.6777777777777778123, 0.6833333333333333481, 0.6888888888888888840, 0.6944444444444444198, 0.6999999999999999556, 0.7055555555555556024, 0.7111111111111111382, 0.7166666666666666741, 0.7222222222222222099, 0.7277777777777777457, 0.7333333333333332815, 0.7388888888888889284, 0.7444444444444444642, 0.7500000000000000000, 0.7555555555555555358, 0.7611111111111110716, 0.7666666666666667185, 0.7722222222222222543, 0.7777777777777777901, 0.7833333333333333259, 0.7888888888888888618, 0.7944444444444443976, 0.8000000000000000444, 0.8055555555555555802, 0.8111111111111111160, 0.8166666666666666519, 0.8222222222222221877, 0.8277777777777777235, 0.8333333333333333703, 0.8388888888888889062, 0.8444444444444444420, 0.8499999999999999778, 0.8555555555555555136, 0.8611111111111111605, 0.8666666666666666963, 0.8722222222222222321, 0.8777777777777777679, 0.8833333333333333037, 0.8888888888888888395, 0.8944444444444444864, 0.9000000000000000222, 0.9055555555555555580, 0.9111111111111110938, 0.9166666666666666297, 0.9222222222222222765, 0.9277777777777778123, 0.9333333333333333481, 0.9388888888888888840, 0.9444444444444444198, 0.9499999999999999556, 0.9555555555555556024, 0.9611111111111111382, 0.9666666666666666741, 0.9722222222222222099, 0.9777777777777777457, 0.9814746766279994761, 0.9912894233942795008 ),
 .UNSPECIFIED. ) 
 GEOMETRIC_REPRESENTATION_ITEM ( )  RATIONAL_B_SPLINE_SURFACE ( (
 ( 1.000000000000000000, 0.9510565162951535312, 1.000000000000000000, 0.9510565162951535312, 1.000000000000000000, 0.9510565162951535312, 1.000000000000000000, 0.9510565162951535312, 1.000000000000000000, 0.9510565162951535312, 1.000000000000000000, 0.9510565162951535312, 1.000000000000000000, 0.9510565162951535312, 1.000000000000000000, 0.9510565162951535312, 1.000000000000000000, 0.9510565162951535312, 1.000000000000000000, 0.9510565162951535312, 1.000000000000000000, 0.9510565162951535312, 1.000000000000000000, 0.9510565162951535312, 1.000000000000000000, 0.9510565162951535312, 1.000000000000000000, 0.9510565162951535312, 1.000000000000000000, 0.9510565162951535312, 1.000000000000000000, 0.9510565162951535312, 1.000000000000000000, 0.9510565162951535312, 1.000000000000000000, 0.9510565162951535312, 1.000000000000000000, 0.9510565162951535312, 1.000000000000000000, 0.9510565162951535312, 1.000000000000000000, 0.9510565162951535312, 1.000000000000000000, 0.9510565162951535312, 1.000000000000000000, 0.9510565162951535312, 1.000000000000000000, 0.9510565162951535312, 1.000000000000000000, 0.9510565162951535312, 1.000000000000000000, 0.9510565162951535312, 1.000000000000000000, 0.9510565162951535312, 1.000000000000000000, 0.9510565162951535312, 1.000000000000000000, 0.9510565162951535312, 1.000000000000000000, 0.9510565162951535312, 1.000000000000000000, 0.9510565162951535312, 1.000000000000000000, 0.9510565162951535312, 1.000000000000000000, 0.9510565162951535312, 1.000000000000000000, 0.9510565162951535312, 1.000000000000000000, 0.9510565162951535312, 1.000000000000000000, 0.9510565162951535312, 1.000000000000000000, 0.9510565162951535312, 1.000000000000000000, 0.9510565162951535312, 1.000000000000000000, 0.9510565162951535312, 1.000000000000000000, 0.9510565162951535312, 1.000000000000000000, 0.9510565162951535312, 1.000000000000000000, 0.9510565162951535312, 1.000000000000000000, 0.9510565162951535312, 1.000000000000000000, 0.9510565162951535312, 1.000000000000000000, 0.9510565162951535312, 1.000000000000000000, 0.9510565162951535312, 1.000000000000000000, 0.9510565162951535312, 1.000000000000000000, 0.9510565162951535312, 1.000000000000000000, 0.9510565162951535312, 1.000000000000000000, 0.9510565162951535312, 1.000000000000000000, 0.9510565162951535312, 1.000000000000000000, 0.9510565162951535312, 1.000000000000000000, 0.9510565162951535312, 1.000000000000000000, 0.9510565162951535312, 1.000000000000000000, 0.9510565162951535312, 1.000000000000000000, 0.9510565162951535312, 1.000000000000000000, 0.9510565162951535312, 1.000000000000000000, 0.9510565162951535312, 1.000000000000000000, 0.9510565162951535312, 1.000000000000000000, 0.9510565162951535312, 1.000000000000000000, 0.9510565162951535312, 1.000000000000000000, 0.9510565162951535312, 1.000000000000000000, 0.9510565162951535312, 1.000000000000000000, 0.9510565162951535312, 1.000000000000000000, 0.9510565162951535312, 1.000000000000000000, 0.9510565162951535312, 1.000000000000000000, 0.9510565162951535312, 1.000000000000000000, 0.9510565162951535312, 1.000000000000000000, 0.9510565162951535312, 1.000000000000000000, 0.9510565162951535312, 1.000000000000000000, 0.9510565162951535312, 1.000000000000000000, 0.9510565162951535312, 1.000000000000000000, 0.9510565162951535312, 1.000000000000000000, 0.9510565162951535312, 1.000000000000000000, 0.9510565162951535312, 1.000000000000000000, 0.9510565162951535312, 1.000000000000000000, 0.9510565162951535312, 1.000000000000000000, 0.9510565162951535312, 1.000000000000000000, 0.9510565162951535312, 1.000000000000000000, 0.9510565162951535312, 1.000000000000000000, 0.9510565162951535312, 1.000000000000000000, 0.9510565162951535312, 1.000000000000000000, 0.9510565162951535312, 1.000000000000000000, 0.9510565162951535312, 1.000000000000000000, 0.9510565162951535312, 1.000000000000000000, 0.9510565162951535312, 1.000000000000000000, 0.9510565162951535312, 1.000000000000000000, 0.9510565162951535312, 1.000000000000000000, 0.9510565162951535312, 1.000000000000000000, 0.9510565162951535312, 1.000000000000000000, 0.9510565162951535312, 1.000000000000000000, 0.9510565162951535312, 1.000000000000000000, 0.9510565162951535312, 1.000000000000000000, 0.9510565162951535312, 1.000000000000000000, 0.9510565162951535312, 1.000000000000000000, 0.9510565162951535312, 1.000000000000000000, 0.9510565162951535312, 1.000000000000000000, 0.9510565162951535312, 1.000000000000000000, 0.9510565162951535312, 1.000000000000000000, 0.9510565162951535312, 1.000000000000000000, 0.9510565162951535312, 1.000000000000000000, 0.9510565162951535312, 1.000000000000000000, 0.9510565162951535312, 1.000000000000000000, 0.9510565162951535312, 1.000000000000000000, 0.9510565162951535312, 1.000000000000000000, 0.9510565162951535312, 1.000000000000000000, 0.9510565162951535312, 1.000000000000000000, 0.9510565162951535312, 1.000000000000000000, 0.9510565162951535312, 1.000000000000000000, 0.9510565162951535312, 1.000000000000000000, 0.9510565162951535312, 1.000000000000000000, 0.9510565162951535312, 1.000000000000000000, 0.9510565162951535312, 1.000000000000000000, 0.9510565162951535312, 1.000000000000000000, 0.9510565162951535312, 1.000000000000000000, 0.9510565162951535312, 1.000000000000000000, 0.9510565162951535312, 1.000000000000000000, 0.9510565162951535312, 1.000000000000000000, 0.9510565162951535312, 1.000000000000000000, 0.9510565162951535312, 1.000000000000000000, 0.9510565162951535312, 1.000000000000000000, 0.9510565162951535312, 1.000000000000000000, 0.9510565162951535312, 1.000000000000000000, 0.9510565162951535312, 1.000000000000000000, 0.9510565162951535312, 1.000000000000000000, 0.9510565162951535312, 1.000000000000000000, 0.9510565162951535312, 1.000000000000000000, 0.9510565162951535312, 1.000000000000000000, 0.9510565162951535312, 1.000000000000000000, 0.9510565162951535312, 1.000000000000000000, 0.9510565162951535312, 1.000000000000000000, 0.9510565162951535312, 1.000000000000000000, 0.9510565162951535312, 1.000000000000000000, 0.9510565162951535312, 1.000000000000000000, 0.9510565162951535312, 1.000000000000000000, 0.9510565162951535312, 1.000000000000000000, 0.9510565162951535312, 1.000000000000000000, 0.9510565162951535312, 1.000000000000000000, 0.9510565162951535312, 1.000000000000000000, 0.9510565162951535312, 1.000000000000000000, 0.9510565162951535312, 1.000000000000000000, 0.9510565162951535312, 1.000000000000000000, 0.9510565162951535312, 1.000000000000000000, 0.9510565162951535312, 1.000000000000000000, 0.9510565162951535312, 1.000000000000000000, 0.9510565162951535312, 1.000000000000000000, 0.9510565162951535312, 1.000000000000000000, 0.9510565162951535312, 1.000000000000000000, 0.9510565162951535312, 1.000000000000000000, 0.9510565162951535312, 1.000000000000000000, 0.9510565162951535312, 1.000000000000000000, 0.9510565162951535312, 1.000000000000000000, 0.9510565162951535312, 1.000000000000000000, 0.9510565162951535312, 1.000000000000000000, 0.9510565162951535312, 1.000000000000000000, 0.9510565162951535312, 1.000000000000000000, 0.9510565162951535312, 1.000000000000000000, 0.9510565162951535312, 1.000000000000000000, 0.9510565162951535312, 1.000000000000000000, 0.9510565162951535312, 1.000000000000000000, 0.9510565162951535312, 1.000000000000000000, 0.9510565162951535312, 1.000000000000000000, 0.9510565162951535312, 1.000000000000000000, 0.9510565162951535312, 1.000000000000000000, 0.9510565162951535312, 1.000000000000000000, 0.9510565162951535312, 1.000000000000000000, 0.9510565162951535312, 1.000000000000000000, 0.9510565162951535312, 1.000000000000000000, 0.9510565162951535312, 1.000000000000000000, 0.9510565162951535312, 1.000000000000000000, 0.9510565162951535312, 1.000000000000000000, 0.9510565162951535312, 1.000000000000000000, 0.9510565162951535312, 1.000000000000000000, 0.9510565162951535312, 1.000000000000000000, 0.9510565162951535312, 1.000000000000000000, 0.9510565162951535312, 1.000000000000000000, 0.9674309604458272149, 0.9782075210486875783, 0.9782075210486875783, 0.9782075210486875783),
 ( 1.000000000000000000, 0.9510565162951535312, 1.000000000000000000, 0.9510565162951535312, 1.000000000000000000, 0.9510565162951535312, 1.000000000000000000, 0.9510565162951535312, 1.000000000000000000, 0.9510565162951535312, 1.000000000000000000, 0.9510565162951535312, 1.000000000000000000, 0.9510565162951535312, 1.000000000000000000, 0.9510565162951535312, 1.000000000000000000, 0.9510565162951535312, 1.000000000000000000, 0.9510565162951535312, 1.000000000000000000, 0.9510565162951535312, 1.000000000000000000, 0.9510565162951535312, 1.000000000000000000, 0.9510565162951535312, 1.000000000000000000, 0.9510565162951535312, 1.000000000000000000, 0.9510565162951535312, 1.000000000000000000, 0.9510565162951535312, 1.000000000000000000, 0.9510565162951535312, 1.000000000000000000, 0.9510565162951535312, 1.000000000000000000, 0.9510565162951535312, 1.000000000000000000, 0.9510565162951535312, 1.000000000000000000, 0.9510565162951535312, 1.000000000000000000, 0.9510565162951535312, 1.000000000000000000, 0.9510565162951535312, 1.000000000000000000, 0.9510565162951535312, 1.000000000000000000, 0.9510565162951535312, 1.000000000000000000, 0.9510565162951535312, 1.000000000000000000, 0.9510565162951535312, 1.000000000000000000, 0.9510565162951535312, 1.000000000000000000, 0.9510565162951535312, 1.000000000000000000, 0.9510565162951535312, 1.000000000000000000, 0.9510565162951535312, 1.000000000000000000, 0.9510565162951535312, 1.000000000000000000, 0.9510565162951535312, 1.000000000000000000, 0.9510565162951535312, 1.000000000000000000, 0.9510565162951535312, 1.000000000000000000, 0.9510565162951535312, 1.000000000000000000, 0.9510565162951535312, 1.000000000000000000, 0.9510565162951535312, 1.000000000000000000, 0.9510565162951535312, 1.000000000000000000, 0.9510565162951535312, 1.000000000000000000, 0.9510565162951535312, 1.000000000000000000, 0.9510565162951535312, 1.000000000000000000, 0.9510565162951535312, 1.000000000000000000, 0.9510565162951535312, 1.000000000000000000, 0.9510565162951535312, 1.000000000000000000, 0.9510565162951535312, 1.000000000000000000, 0.9510565162951535312, 1.000000000000000000, 0.9510565162951535312, 1.000000000000000000, 0.9510565162951535312, 1.000000000000000000, 0.9510565162951535312, 1.000000000000000000, 0.9510565162951535312, 1.000000000000000000, 0.9510565162951535312, 1.000000000000000000, 0.9510565162951535312, 1.000000000000000000, 0.9510565162951535312, 1.000000000000000000, 0.9510565162951535312, 1.000000000000000000, 0.9510565162951535312, 1.000000000000000000, 0.9510565162951535312, 1.000000000000000000, 0.9510565162951535312, 1.000000000000000000, 0.9510565162951535312, 1.000000000000000000, 0.9510565162951535312, 1.000000000000000000, 0.9510565162951535312, 1.000000000000000000, 0.9510565162951535312, 1.000000000000000000, 0.9510565162951535312, 1.000000000000000000, 0.9510565162951535312, 1.000000000000000000, 0.9510565162951535312, 1.000000000000000000, 0.9510565162951535312, 1.000000000000000000, 0.9510565162951535312, 1.000000000000000000, 0.9510565162951535312, 1.000000000000000000, 0.9510565162951535312, 1.000000000000000000, 0.9510565162951535312, 1.000000000000000000, 0.9510565162951535312, 1.000000000000000000, 0.9510565162951535312, 1.000000000000000000, 0.9510565162951535312, 1.000000000000000000, 0.9510565162951535312, 1.000000000000000000, 0.9510565162951535312, 1.000000000000000000, 0.9510565162951535312, 1.000000000000000000, 0.9510565162951535312, 1.000000000000000000, 0.9510565162951535312, 1.000000000000000000, 0.9510565162951535312, 1.000000000000000000, 0.9510565162951535312, 1.000000000000000000, 0.9510565162951535312, 1.000000000000000000, 0.9510565162951535312, 1.000000000000000000, 0.9510565162951535312, 1.000000000000000000, 0.9510565162951535312, 1.000000000000000000, 0.9510565162951535312, 1.000000000000000000, 0.9510565162951535312, 1.000000000000000000, 0.9510565162951535312, 1.000000000000000000, 0.9510565162951535312, 1.000000000000000000, 0.9510565162951535312, 1.000000000000000000, 0.9510565162951535312, 1.000000000000000000, 0.9510565162951535312, 1.000000000000000000, 0.9510565162951535312, 1.000000000000000000, 0.9510565162951535312, 1.000000000000000000, 0.9510565162951535312, 1.000000000000000000, 0.9510565162951535312, 1.000000000000000000, 0.9510565162951535312, 1.000000000000000000, 0.9510565162951535312, 1.000000000000000000, 0.9510565162951535312, 1.000000000000000000, 0.9510565162951535312, 1.000000000000000000, 0.9510565162951535312, 1.000000000000000000, 0.9510565162951535312, 1.000000000000000000, 0.9510565162951535312, 1.000000000000000000, 0.9510565162951535312, 1.000000000000000000, 0.9510565162951535312, 1.000000000000000000, 0.9510565162951535312, 1.000000000000000000, 0.9510565162951535312, 1.000000000000000000, 0.9510565162951535312, 1.000000000000000000, 0.9510565162951535312, 1.000000000000000000, 0.9510565162951535312, 1.000000000000000000, 0.9510565162951535312, 1.000000000000000000, 0.9510565162951535312, 1.000000000000000000, 0.9510565162951535312, 1.000000000000000000, 0.9510565162951535312, 1.000000000000000000, 0.9510565162951535312, 1.000000000000000000, 0.9510565162951535312, 1.000000000000000000, 0.9510565162951535312, 1.000000000000000000, 0.9510565162951535312, 1.000000000000000000, 0.9510565162951535312, 1.000000000000000000, 0.9510565162951535312, 1.000000000000000000, 0.9510565162951535312, 1.000000000000000000, 0.9510565162951535312, 1.000000000000000000, 0.9510565162951535312, 1.000000000000000000, 0.9510565162951535312, 1.000000000000000000, 0.9510565162951535312, 1.000000000000000000, 0.9510565162951535312, 1.000000000000000000, 0.9510565162951535312, 1.000000000000000000, 0.9510565162951535312, 1.000000000000000000, 0.9510565162951535312, 1.000000000000000000, 0.9510565162951535312, 1.000000000000000000, 0.9510565162951535312, 1.000000000000000000, 0.9510565162951535312, 1.000000000000000000, 0.9510565162951535312, 1.000000000000000000, 0.9510565162951535312, 1.000000000000000000, 0.9510565162951535312, 1.000000000000000000, 0.9510565162951535312, 1.000000000000000000, 0.9510565162951535312, 1.000000000000000000, 0.9510565162951535312, 1.000000000000000000, 0.9510565162951535312, 1.000000000000000000, 0.9510565162951535312, 1.000000000000000000, 0.9510565162951535312, 1.000000000000000000, 0.9510565162951535312, 1.000000000000000000, 0.9510565162951535312, 1.000000000000000000, 0.9510565162951535312, 1.000000000000000000, 0.9510565162951535312, 1.000000000000000000, 0.9510565162951535312, 1.000000000000000000, 0.9510565162951535312, 1.000000000000000000, 0.9510565162951535312, 1.000000000000000000, 0.9510565162951535312, 1.000000000000000000, 0.9510565162951535312, 1.000000000000000000, 0.9510565162951535312, 1.000000000000000000, 0.9510565162951535312, 1.000000000000000000, 0.9510565162951535312, 1.000000000000000000, 0.9510565162951535312, 1.000000000000000000, 0.9510565162951535312, 1.000000000000000000, 0.9510565162951535312, 1.000000000000000000, 0.9510565162951535312, 1.000000000000000000, 0.9510565162951535312, 1.000000000000000000, 0.9510565162951535312, 1.000000000000000000, 0.9510565162951535312, 1.000000000000000000, 0.9510565162951535312, 1.000000000000000000, 0.9510565162951535312, 1.000000000000000000, 0.9510565162951535312, 1.000000000000000000, 0.9510565162951535312, 1.000000000000000000, 0.9510565162951535312, 1.000000000000000000, 0.9510565162951535312, 1.000000000000000000, 0.9510565162951535312, 1.000000000000000000, 0.9510565162951535312, 1.000000000000000000, 0.9510565162951535312, 1.000000000000000000, 0.9510565162951535312, 1.000000000000000000, 0.9510565162951535312, 1.000000000000000000, 0.9510565162951535312, 1.000000000000000000, 0.9510565162951535312, 1.000000000000000000, 0.9510565162951535312, 1.000000000000000000, 0.9510565162951535312, 1.000000000000000000, 0.9510565162951535312, 1.000000000000000000, 0.9510565162951535312, 1.000000000000000000, 0.9674309604458272149, 0.9782075210486875783, 0.9782075210486875783, 0.9782075210486875783) ) ) 
 REPRESENTATION_ITEM ( '' )  SURFACE ( )  );
#1475 = CARTESIAN_POINT ( 'NONE',  ( 4.171729424061789260, 71.82999999999999829, 12.83926296998457417 ) ) ;
#1476 = CARTESIAN_POINT ( 'NONE',  ( -11.66078065398632191, 52.67688486108551160, -6.805658509415644097 ) ) ;
#1477 = AXIS2_PLACEMENT_3D ( 'NONE', #16468, #5800, #3117 ) ;
#1478 = CARTESIAN_POINT ( 'NONE',  ( -7.576616670048093940E-16, 45.67999999999999261, 12.37355403259654985 ) ) ;
#1479 = CARTESIAN_POINT ( 'NONE',  ( 4.171729424061791924, 63.03000000000000114, -12.83926296998457239 ) ) ;
#1480 = CARTESIAN_POINT ( 'NONE',  ( -17.14741290055372147, 7.815224843475952810, -8.000000000000202505 ) ) ;
#1481 = CARTESIAN_POINT ( 'NONE',  ( 13.41380563842359486, 69.37697373310895443, 1.523135287452938691 ) ) ;
#1482 = CARTESIAN_POINT ( 'NONE',  ( -4.726456801501960570, 37.35019383979712870, -12.64734214246707822 ) ) ;
#1483 = CARTESIAN_POINT ( 'NONE',  ( 13.50017362217845118, 36.42540073931617428, 0.1282887782157201839 ) ) ;
#1484 = CARTESIAN_POINT ( 'NONE',  ( 18.62500000000000000, -40.54999999999992610, 1.560692158462880521E-12 ) ) ;
#1485 = CARTESIAN_POINT ( 'NONE',  ( -12.08134441457838371, 74.15176713050708202, 6.024497238434195268 ) ) ;
#1486 = CARTESIAN_POINT ( 'NONE',  ( -13.29890090237351608, 76.84837936454550800, -2.321472569501058292 ) ) ;
#1487 = AXIS2_PLACEMENT_3D ( 'NONE', #5312, #5135, #10525 ) ;
#1488 = EDGE_CURVE ( 'NONE', #17140, #14888, #10411, .T. ) ;
#1489 = CARTESIAN_POINT ( 'NONE',  ( -12.38400671196816383, 79.73365040721881769, -5.379209168480316272 ) ) ;
#1490 = CARTESIAN_POINT ( 'NONE',  ( -0.7362654489766442545, 80.93000000000003524, 13.00758670406994355 ) ) ;
#1491 = FACE_OUTER_BOUND ( 'NONE', #16923, .T. ) ;
#1492 = CARTESIAN_POINT ( 'NONE',  ( 11.76794919243112680, 5.580000000000004512, -3.823638476888993942 ) ) ;
#1493 = CARTESIAN_POINT ( 'NONE',  ( 3.636496289402157078, 50.03000000000000114, -11.19198476289190936 ) ) ;
#1494 = CARTESIAN_POINT ( 'NONE',  ( -18.62499999999934985, -23.93437499999993889, -7.714727599200458918 ) ) ;
#1495 = CARTESIAN_POINT ( 'NONE',  ( -13.49999999999999822, -15.91999999999999815, 4.386415899144235908 ) ) ;
#1496 = DIRECTION ( 'NONE',  ( 0.8660254037844430375, 0.000000000000000000, -0.4999999999999925060 ) ) ;
#1497 = CARTESIAN_POINT ( 'NONE',  ( 11.38591239875901273, 75.15846830473550710, 7.253424416596073954 ) ) ;
#1498 = CARTESIAN_POINT ( 'NONE',  ( 13.94865728765873492, -5.025561147604149903E-16, -11.57659991980615644 ) ) ;
#1499 = CARTESIAN_POINT ( 'NONE',  ( 11.76794919243112325, 31.42999999999999972, 1.441158131103945434E-15 ) ) ;
#1500 = CARTESIAN_POINT ( 'NONE',  ( -8.136154617392147514, 41.37131206498728631, 10.78203447320519182 ) ) ;
#1501 = CARTESIAN_POINT ( 'NONE',  ( -6.420066188578533506, 58.41575564973159373, -11.88523871910323670 ) ) ;
#1502 = CARTESIAN_POINT ( 'NONE',  ( 4.399052845997258210, 44.83819265409231036, 12.76382163886394672 ) ) ;
#1503 = DIRECTION ( 'NONE',  ( 0.000000000000000000, 1.000000000000000000, 0.000000000000000000 ) ) ;
#1504 = FACE_OUTER_BOUND ( 'NONE', #15495, .T. ) ;
#1505 = DIRECTION ( 'NONE',  ( 0.000000000000000000, 0.000000000000000000, -1.000000000000000000 ) ) ;
#1506 = CARTESIAN_POINT ( 'NONE',  ( -8.651203465105309576, 49.51225507058038744, -10.37610565160799858 ) ) ;
#1507 = CARTESIAN_POINT ( 'NONE',  ( 11.51013096457343110, 63.69335374111208381, -7.054565399514032720 ) ) ;
#1508 = CARTESIAN_POINT ( 'NONE',  ( 10.57057823592805335, 42.11001419281064528, 8.397306183127296819 ) ) ;
#1509 = CARTESIAN_POINT ( 'NONE',  ( 4.962292416515707849, 38.85892357782116591, 12.55684533990331175 ) ) ;
#1510 = ORIENTED_EDGE ( 'NONE', *, *, #617, .F. ) ;
#1511 = CARTESIAN_POINT ( 'NONE',  ( -3.961846529824640584, 70.32245338488193909, -12.90557292749110019 ) ) ;
#1512 = CARTESIAN_POINT ( 'NONE',  ( -8.043339635997654113, -10.40624999999997513, 8.043339635996302306 ) ) ;
#1513 = ORIENTED_EDGE ( 'NONE', *, *, #13823, .F. ) ;
#1514 = CARTESIAN_POINT ( 'NONE',  ( -2.416183868245585842, 43.26687697742507055, -13.28262826839602084 ) ) ;
#1515 = CARTESIAN_POINT ( 'NONE',  ( -25.42428528562860279, 0.000000000000000000, 5.441113646577211860 ) ) ;
#1516 = CARTESIAN_POINT ( 'NONE',  ( 6.542732549386596652, 60.93925339870889957, -11.80881426700419468 ) ) ;
#1517 = CARTESIAN_POINT ( 'NONE',  ( -8.343458848123576743, 8.480000000000000426, -11.48378591275254301 ) ) ;
#1518 = CARTESIAN_POINT ( 'NONE',  ( -18.62499999999935341, -23.93437499999994245, -7.714727599200458918 ) ) ;
#1519 = CARTESIAN_POINT ( 'NONE',  ( 13.10901505835366265, 66.54634616873129005, -3.274170164232866664 ) ) ;
#1520 = CARTESIAN_POINT ( 'NONE',  ( 4.906913175764546331, 56.85693511058605765, 12.57669196521769095 ) ) ;
#1521 = CARTESIAN_POINT ( 'NONE',  ( 7.272992578804311492, 58.88000000000000256, -10.01041549318726709 ) ) ;
#1522 = CARTESIAN_POINT ( 'NONE',  ( 11.76794919243112325, 70.28000000000000114, 3.823638476888996607 ) ) ;
#1523 = CARTESIAN_POINT ( 'NONE',  ( -8.816587287286456132, 47.33998666666719402, 10.23251018546078583 ) ) ;
#1524 = ADVANCED_FACE ( 'NONE', ( #13135, #17104 ), #5011, .F. ) ;
#1525 = DIRECTION ( 'NONE',  ( -8.379555213223520053E-14, 0.000000000000000000, 1.000000000000000000 ) ) ;
#1526 = CARTESIAN_POINT ( 'NONE',  ( 3.708203932499389843, 9.163974596215608059, -11.41267819554190233 ) ) ;
#1527 = CARTESIAN_POINT ( 'NONE',  ( 5.004910567252390585, -99.99999999999995737, 15.37359115544943577 ) ) ;
#1528 = CARTESIAN_POINT ( 'NONE',  ( -7.972521863940812636, 56.37881760393914021, 10.91819665946111151 ) ) ;
#1529 = CARTESIAN_POINT ( 'NONE',  ( -11.37499999999960387, -90.53437499999978400, -4.711679271994910323 ) ) ;
#1530 = DIRECTION ( 'NONE',  ( -0.000000000000000000, 1.000000000000000000, -0.000000000000000000 ) ) ;
#1531 = CIRCLE ( 'NONE', #9464, 6.000000000000000000 ) ;
#1532 = CARTESIAN_POINT ( 'NONE',  ( 11.22862360393084202, 33.71149563479018241, -7.494544542091995609 ) ) ;
#1533 = CARTESIAN_POINT ( 'NONE',  ( -9.869785582228594478, 9.999999999999998224, 7.125699818525842666 ) ) ;
#1534 = CARTESIAN_POINT ( 'NONE',  ( -9.354252080082858356, 8.052096965364873071, -15.42305849549719454 ) ) ;
#1535 = ORIENTED_EDGE ( 'NONE', *, *, #4716, .F. ) ;
#1536 = CARTESIAN_POINT ( 'NONE',  ( -3.886324430026127708, 62.54026215031276337, 12.92852040802742053 ) ) ;
#1537 = ORIENTED_EDGE ( 'NONE', *, *, #4951, .F. ) ;
#1538 = CARTESIAN_POINT ( 'NONE',  ( -7.714727599197334307, -29.10312499999994884, -18.62500000000064659 ) ) ;
#1539 = CARTESIAN_POINT ( 'NONE',  ( -13.25829652241704970, 44.01964385073794261, 2.543230693382868335 ) ) ;
#1540 = CARTESIAN_POINT ( 'NONE',  ( -9.152478727637712197, 8.062211461649205546, 15.50029318102135356 ) ) ;
#1541 = CARTESIAN_POINT ( 'NONE',  ( -8.343458848123576743, 31.47999999999999687, -11.48378591275254301 ) ) ;
#1542 = CARTESIAN_POINT ( 'NONE',  ( 8.343458848123578520, 46.97999999999998977, 11.48378591275254124 ) ) ;
#1543 = CARTESIAN_POINT ( 'NONE',  ( -13.48705080653788002, 70.90931382874535416, -0.6006972830549630604 ) ) ;
#1544 = CARTESIAN_POINT ( 'NONE',  ( 18.62499999999935341, -41.65937499999989058, 7.714727599200469577 ) ) ;
#1545 = CARTESIAN_POINT ( 'NONE',  ( -2.845161873668661023, 67.28236192527593573, -13.19680914032984553 ) ) ;
#1546 = CARTESIAN_POINT ( 'NONE',  ( -18.62500000000064659, -85.36562499999978115, 7.714727599197333419 ) ) ;
#1547 = CARTESIAN_POINT ( 'NONE',  ( 13.06806765790989822, 54.30935285006482616, 3.387711129923342668 ) ) ;
#1548 = CARTESIAN_POINT ( 'NONE',  ( -3.636496289402152637, 15.33000000000001073, -11.19198476289190936 ) ) ;
#1549 = CARTESIAN_POINT ( 'NONE',  ( -3.720992066526385145, 64.31351913756894589, -12.97891995391547404 ) ) ;
#1550 = ORIENTED_EDGE ( 'NONE', *, *, #498, .T. ) ;
#1551 = CARTESIAN_POINT ( 'NONE',  ( -13.31284211965473219, 35.00873797297208512, 2.241149820570724760 ) ) ;
#1552 = ORIENTED_EDGE ( 'NONE', *, *, #5033, .F. ) ;
#1553 = CARTESIAN_POINT ( 'NONE',  ( 13.41149850370572238, 78.37616975112200635, 1.543702408172776375 ) ) ;
#1554 = CARTESIAN_POINT ( 'NONE',  ( -2.229658519546948270, -3.026718717157248455E-15, -12.03768796296077248 ) ) ;
#1555 = CARTESIAN_POINT ( 'NONE',  ( -10.99999999999979394, 0.000000000000000000, -15.58845726812003996 ) ) ;
#1556 = CARTESIAN_POINT ( 'NONE',  ( 7.500000000000002665, -25.82163707610023096, 7.534909587719538671 ) ) ;
#1557 = CARTESIAN_POINT ( 'NONE',  ( 11.12432746466444478, 72.71790841392339644, -7.648681935121548925 ) ) ;
#1558 = CARTESIAN_POINT ( 'NONE',  ( 6.558562036928162087, 59.92140053412916245, 11.79980395858304298 ) ) ;
#1559 = CARTESIAN_POINT ( 'NONE',  ( -10.92172942406179104, -14.76999999999999780, 7.935100905948385908 ) ) ;
#1560 = VECTOR ( 'NONE', #15768, 1000.000000000000000 ) ;
#1561 = CARTESIAN_POINT ( 'NONE',  ( 13.49999999999999822, 75.28000000000000114, 4.386415899144237684 ) ) ;
#1562 = CARTESIAN_POINT ( 'NONE',  ( -13.47525611461717610, 52.90179884393261034, -0.8176782787010556941 ) ) ;
#1563 = CARTESIAN_POINT ( 'NONE',  ( 9.520470885617715595, 49.13000000000000256, 6.917026985038134512 ) ) ;
#1564 = CARTESIAN_POINT ( 'NONE',  ( 13.50000000000000355, 62.57999999999999119, -4.386415899144233244 ) ) ;
#1565 = ADVANCED_FACE ( 'NONE', ( #9091, #14444 ), #2980, .F. ) ;
#1566 = CARTESIAN_POINT ( 'NONE',  ( 1.689034877922362510, 50.74073306604915246, 13.39397960069070059 ) ) ;
#1567 = CARTESIAN_POINT ( 'NONE',  ( 7.506036428011613637, 68.96118737518608555, 11.22175974229874562 ) ) ;
#1568 = CARTESIAN_POINT ( 'NONE',  ( 2.222800136090958861E-15, 3.313974596215566670, -12.00000000000000355 ) ) ;
#1569 = CARTESIAN_POINT ( 'NONE',  ( 12.00000000000000355, 5.446025403784441998, -3.899036354794874093 ) ) ;
#1570 = CARTESIAN_POINT ( 'NONE',  ( 4.711679271993006957, -104.0281249999997755, 11.37500000000039257 ) ) ;
#1571 = CARTESIAN_POINT ( 'NONE',  ( -13.03759029931439350, 74.05493905520845033, 3.503315162420880924 ) ) ;
#1572 = VECTOR ( 'NONE', #14237, 1000.000000000000000 ) ;
#1573 = CARTESIAN_POINT ( 'NONE',  ( -13.03456398638965119, 76.80422654878610444, -3.523612153066970620 ) ) ;
#1574 = CARTESIAN_POINT ( 'NONE',  ( -2.011276037618017209, 79.25206798469932323, -13.37631185983492799 ) ) ;
#1575 = CARTESIAN_POINT ( 'NONE',  ( -12.00000000000000178, 0.6460254037844337383, -3.899036354794879422 ) ) ;
#1576 = FACE_OUTER_BOUND ( 'NONE', #7475, .T. ) ;
#1577 = CARTESIAN_POINT ( 'NONE',  ( 8.343458848123583849, 31.87999999999999901, -11.48378591275253768 ) ) ;
#1578 = CARTESIAN_POINT ( 'NONE',  ( 3.636496289402154414, -10.16999999999999815, 11.19198476289190758 ) ) ;
#1579 = CARTESIAN_POINT ( 'NONE',  ( 11.76794919243112325, 46.42999999999999972, 1.441158131103945434E-15 ) ) ;
#1580 = CARTESIAN_POINT ( 'NONE',  ( -8.549982208541774191E-16, -15.32000000000000384, 14.19474002721660355 ) ) ;
#1581 = CARTESIAN_POINT ( 'NONE',  ( 13.50000000000000355, 35.57999999999999829, -4.386415899144233244 ) ) ;
#1582 = CARTESIAN_POINT ( 'NONE',  ( 13.26855327705798615, 75.34217119327314549, 2.493469984181274857 ) ) ;
#1583 = CARTESIAN_POINT ( 'NONE',  ( 6.913829868824056035, -7.609836600491605532E-16, -10.40368044132385528 ) ) ;
#1584 = AXIS2_PLACEMENT_3D ( 'NONE', #6330, #11719, #17184 ) ;
#1585 = CARTESIAN_POINT ( 'NONE',  ( 7.500000000000000000, -28.00000000000000000, -9.367496997597600128 ) ) ;
#1586 = CARTESIAN_POINT ( 'NONE',  ( -11.16325391095078601, 41.21556957424302681, 7.591565366864450048 ) ) ;
#1587 = EDGE_CURVE ( 'NONE', #17275, #11330, #7247, .T. ) ;
#1588 = CARTESIAN_POINT ( 'NONE',  ( 4.626088177006855595, 52.01347804022521615, -12.68284349646924092 ) ) ;
#1589 = CARTESIAN_POINT ( 'NONE',  ( 1.156423937993576345, 44.72144737391447222, 13.45781478867673897 ) ) ;
#1590 = CARTESIAN_POINT ( 'NONE',  ( 0.000000000000000000, 80.93000000000000682, -12.00000000000000178 ) ) ;
#1591 = CARTESIAN_POINT ( 'NONE',  ( -2.138189944381236884, 4.256881422320271113, -13.50000000000000000 ) ) ;
#1592 = CARTESIAN_POINT ( 'NONE',  ( -2.734444271416374749E-11, 0.3139745962166686777, -12.00000000000000000 ) ) ;
#1593 = CARTESIAN_POINT ( 'NONE',  ( -12.15092532215536636, 49.71386956109132171, -5.882865350636430790 ) ) ;
#1594 = CARTESIAN_POINT ( 'NONE',  ( 10.65813095105755970, 63.11492048044581082, 8.285788074620803911 ) ) ;
#1595 = B_SPLINE_CURVE_WITH_KNOTS ( 'NONE', 3,
 ( #17292, #9278, #7859, #13150, #9011, #13234, #10337, #11914, #5024, #6358, #3692, #4938, #15957, #5295, #13317, #15692, #14368, #1122, #858, #11831, #14458, #5205, #14630, #17119, #3598, #10423, #3863, #16043, #7684, #9192, #6535, #9105, #11655, #2345, #1209, #17209, #10595, #17033, #6618, #2256, #1038, #2515, #3951, #3780, #7777, #7944, #9364, #6446, #11998, #17380, #11741, #10677, #14714, #15783, #7597, #12975, #5119, #6268, #14541, #13063, #945, #10511, #15873, #2428, #11114, #14886, #9802, #15060, #16125, #12170, #9627, #241, #1288, #13399, #6702, #4214, #2958, #12081, #8121, #17462, #324, #1551, #61, #4302, #8211, #1640, #4036, #13488, #2869, #5465, #10847, #7057, #16215, #1376, #12438, #2781, #4126, #16400, #6790, #9539, #9450, #16486, #14977, #6970, #13573, #12348, #2602, #8301, #6884, #4392, #5377, #14799, #1465, #151, #13741, #10762, #2690, #13657, #5647, #12256, #5557, #10941, #16306, #11028, #5733, #8387, #9714, #8033, #16663, #3046, #15148, #11286, #4657, #501, #11203, #8476, #15499, #16578, #7224, #13827, #5907, #13916, #12698, #16840, #4483, #4571, #12610, #9978, #10065, #1727, #7141, #12786, #15325, #411, #3229, #14003, #8649, #4744, #7405, #1980, #1896, #10148, #7313, #12527, #3411, #672, #5819, #585, #5996, #11378, #9892, #15240, #16750, #6085, #11464, #15415, #1810, #3321, #3138, #8736, #8563, #14095, #3979, #16337, #10877, #91, #12287, #12375, #2809, #13683, #4244, #9654, #9307 ),
 .UNSPECIFIED., .F., .F.,
 ( 4, 2, 1, 1, 2, 2, 1, 2, 2, 2, 2, 1, 2, 2, 1, 2, 2, 2, 1, 2, 2, 1, 2, 2, 1, 1, 1, 2, 2, 1, 1, 2, 2, 2, 2, 2, 1, 1, 1, 1, 2, 2, 2, 1, 1, 2, 2, 2, 2, 2, 2, 1, 1, 2, 2, 1, 1, 2, 2, 2, 1, 2, 2, 1, 2, 2, 2, 2, 2, 2, 2, 2, 2, 1, 2, 2, 1, 1, 1, 1, 2, 2, 1, 2, 2, 1, 1, 1, 2, 2, 2, 2, 1, 1, 2, 2, 2, 2, 2, 1, 1, 2, 2, 1, 1, 2, 2, 2, 2, 2, 1, 1, 2, 2, 2, 2, 4 ),
 ( 0.8872638927956195687, 0.8881829932133823435, 0.8882978807656026765, 0.8883553245417128430, 0.8883696854857403569, 0.8883840464297679818, 0.8884127683178230095, 0.8886425434222637865, 0.8891020936311452294, 0.8900211940489080042, 0.8902509691533487812, 0.8903658567055691142, 0.8903945785936241419, 0.8904233004816792807, 0.8904807442577894472, 0.8909402944666708901, 0.8918593948844337760, 0.8923189450933152189, 0.8923763888694253854, 0.8924051107574805242, 0.8924338326455355519, 0.8925487201977559959, 0.8927784953021966619, 0.8936975957199596587, 0.8941571459288411017, 0.8943869210332818787, 0.8944443648093920451, 0.8944587257534195590, 0.8944659062254333159, 0.8944730866974471839, 0.8945018085855022116, 0.8946166961377225446, 0.8955357965554855415, 0.8964548969732485384, 0.8964836188613036771, 0.8964907993333174341, 0.8964979798053311910, 0.8965123407493587049, 0.8965697845254688714, 0.8966846720776892044, 0.8969144471821298703, 0.8973739973910110912, 0.8982930978087736440, 0.8984079853609939770, 0.8984654291371041435, 0.8984941510251591712, 0.8985228729132143100, 0.8987526480176549759, 0.8992121982265361968, 0.9001312986442987496, 0.9003610737487394156, 0.9004759613009596375, 0.9005334050770698040, 0.9005477660210974289, 0.9005549464931111858, 0.9005621269651249428, 0.9005908488531799705, 0.9010503990620614134, 0.9019694994798241883, 0.9024290496887056312, 0.9025439372409259642, 0.9025726591289811029, 0.9026013810170361307, 0.9026588247931462972, 0.9028885998975869631, 0.9038077003153497380, 0.9042672505242311809, 0.9044970256286718469, 0.9045544694047820133, 0.9046119131808921798, 0.9047268007331125128, 0.9056459011508752877, 0.9065650015686380625, 0.9066224453447482290, 0.9066368062887758539, 0.9066439867607896108, 0.9066511672328033677, 0.9066798891208585065, 0.9067947766730788395, 0.9070245517775195054, 0.9074841019864009484, 0.9084032024041638342, 0.9086329775086046112, 0.9086616993966596389, 0.9086688798686735069, 0.9086760603406872638, 0.9086904212847147777, 0.9087478650608250552, 0.9088627526130454992, 0.9093223028219273862, 0.9102414032396911603, 0.9104711783441321593, 0.9105860658963526033, 0.9106435096724627698, 0.9106722315605179086, 0.9107009534485730473, 0.9111605036574549343, 0.9120796040752185974, 0.9125391542841004844, 0.9126540418363209284, 0.9127114856124312059, 0.9127186660844449628, 0.9127258465564587198, 0.9127402075004863446, 0.9127689293885414834, 0.9129987044929823714, 0.9134582547018642584, 0.9136880298063051464, 0.9139178049107460344, 0.9143773551196279215, 0.9146071302240688095, 0.9147220177762893645, 0.9147507396643443922, 0.9147794615523995310, 0.9148369053285098085, 0.9157560057462735825, 0.9166751061640373566 ),
 .UNSPECIFIED. ) ;
#1596 = CARTESIAN_POINT ( 'NONE',  ( 13.37184084406137430, 42.36507920723824583, 1.857074438056610433 ) ) ;
#1597 = CARTESIAN_POINT ( 'NONE',  ( 4.259800649283492113, 38.83317359495975296, 12.81031967732963750 ) ) ;
#1598 = ORIENTED_EDGE ( 'NONE', *, *, #15747, .F. ) ;
#1599 = CARTESIAN_POINT ( 'NONE',  ( 2.272985001014427393E-15, 77.17999999999999261, -12.37355403259654807 ) ) ;
#1600 = DIRECTION ( 'NONE',  ( 0.000000000000000000, -1.000000000000000000, 0.000000000000000000 ) ) ;
#1601 = DIRECTION ( 'NONE',  ( 0.000000000000000000, 0.000000000000000000, -1.000000000000000000 ) ) ;
#1602 = CARTESIAN_POINT ( 'NONE',  ( -13.50000000000000000, 7.930000000000006821, -3.469446951953614189E-15 ) ) ;
#1603 = ORIENTED_EDGE ( 'NONE', *, *, #15057, .F. ) ;
#1604 = CARTESIAN_POINT ( 'NONE',  ( -5.745312699652264321, 43.38893832881636570, -12.21663294598238814 ) ) ;
#1605 = CARTESIAN_POINT ( 'NONE',  ( -7.500000000000000000, 106.2113042096659257, 8.086389325435060726 ) ) ;
#1606 = CARTESIAN_POINT ( 'NONE',  ( 9.270367474829679821, 60.81777984582654994, -9.813849793336233418 ) ) ;
#1607 = CARTESIAN_POINT ( 'NONE',  ( 10.92172942406179104, 13.72999999999999154, -7.935100905948385908 ) ) ;
#1608 = LINE ( 'NONE', #1780, #9666 ) ;
#1609 = CARTESIAN_POINT ( 'NONE',  ( 13.44655200584734622, 66.38838457564831685, 1.200152482059077208 ) ) ;
#1610 = CARTESIAN_POINT ( 'NONE',  ( 1.669445390708271804, 56.74002890137526833, 13.39659988532823220 ) ) ;
#1611 = CARTESIAN_POINT ( 'NONE',  ( -9.520470885617715595, 62.63000000000000256, -6.917026985038136289 ) ) ;
#1612 = CARTESIAN_POINT ( 'NONE',  ( -11.76794919243112325, 68.77999999999998693, -3.823638476888998827 ) ) ;
#1613 = ADVANCED_FACE ( 'NONE', ( #9827 ), #13677, .F. ) ;
#1614 = CARTESIAN_POINT ( 'NONE',  ( -13.38138642673853340, 46.86721787022950991, -1.795383226577773828 ) ) ;
#1615 = CARTESIAN_POINT ( 'NONE',  ( -2.138189944381279073, 45.25688142232026934, -13.49999999999998579 ) ) ;
#1616 = CARTESIAN_POINT ( 'NONE',  ( -1.363343349470708815E-11, 9.313974596216114676, -12.00000000000000355 ) ) ;
#1617 = CARTESIAN_POINT ( 'NONE',  ( 5.882695696613415848, 30.96571419329114860, -12.15092755760450594 ) ) ;
#1618 = CARTESIAN_POINT ( 'NONE',  ( -1.553209143042241003, 56.62434124648177658, 13.41219526395410533 ) ) ;
#1619 = CARTESIAN_POINT ( 'NONE',  ( 11.37500000000000000, -49.94999999999988205, 9.531744055041752924E-13 ) ) ;
#1620 = CARTESIAN_POINT ( 'NONE',  ( -8.891200544363830713E-16, 40.67999999999999261, 13.50000000000000000 ) ) ;
#1621 = CARTESIAN_POINT ( 'NONE',  ( 13.29512141749893495, 33.34760041236136630, 2.343023588158895887 ) ) ;
#1622 = CARTESIAN_POINT ( 'NONE',  ( -7.999999999999776179, 7.773118517290098062, -17.32050807568887762 ) ) ;
#1623 = DIRECTION ( 'NONE',  ( -0.4999999999999986677, 0.000000000000000000, -0.8660254037844394848 ) ) ;
#1624 = ORIENTED_EDGE ( 'NONE', *, *, #3286, .F. ) ;
#1625 = CARTESIAN_POINT ( 'NONE',  ( -5.813220906962667023, 62.46839348748255816, 12.18503415927900235 ) ) ;
#1626 = EDGE_LOOP ( 'NONE', ( #8430, #17034, #13447, #11158, #1445, #7828, #14784, #17343, #6290, #8389, #15047, #5250, #10214, #2496, #10921, #9873, #239 ) ) ;
#1627 = CARTESIAN_POINT ( 'NONE',  ( -7.714727599197334307, -45.75312499999991189, -18.62500000000064659 ) ) ;
#1628 = EDGE_CURVE ( 'NONE', #1880, #8869, #15379, .T. ) ;
#1629 = CARTESIAN_POINT ( 'NONE',  ( -11.73445831788195015, 44.17842776096925661, 6.691153486874162226 ) ) ;
#1630 = CARTESIAN_POINT ( 'NONE',  ( 9.832031499013087483, 0.06660297321671654336, 9.434941428760371451 ) ) ;
#1631 = CARTESIAN_POINT ( 'NONE',  ( 8.343458848123583849, 33.87999999999998835, -11.48378591275253768 ) ) ;
#1632 = CARTESIAN_POINT ( 'NONE',  ( 8.343458848123578520, 43.97999999999999687, 11.48378591275254124 ) ) ;
#1633 = CARTESIAN_POINT ( 'NONE',  ( -9.608163084644951724, 46.55906845273868555, -9.483316201871774709 ) ) ;
#1634 = CARTESIAN_POINT ( 'NONE',  ( -10.11174617855943048, 67.58510651382286483, -8.944425511103352378 ) ) ;
#1635 = CARTESIAN_POINT ( 'NONE',  ( -13.16986379960055409, -53.10624999999986073, 13.16986379959834252 ) ) ;
#1636 = CARTESIAN_POINT ( 'NONE',  ( 13.49936567077070571, 54.43455718009003874, -0.1330465375380656678 ) ) ;
#1637 = CARTESIAN_POINT ( 'NONE',  ( -10.37798312408888357, 64.59933206745596124, -8.634316133104666946 ) ) ;
#1638 = ORIENTED_EDGE ( 'NONE', *, *, #6605, .F. ) ;
#1639 = CARTESIAN_POINT ( 'NONE',  ( 15.43183772185602898, 8.055054230040790131, -9.319033143235071037 ) ) ;
#1640 = CARTESIAN_POINT ( 'NONE',  ( -13.34459694652892736, 35.00157342978971542, 2.042509889357819297 ) ) ;
#1641 = AXIS2_PLACEMENT_3D ( 'NONE', #15428, #12801, #849 ) ;
#1642 = ORIENTED_EDGE ( 'NONE', *, *, #9399, .F. ) ;
#1643 = CARTESIAN_POINT ( 'NONE',  ( 11.86781241222626804, 78.19182051743750606, 6.434699402502147336 ) ) ;
#1644 = LINE ( 'NONE', #16667, #16889 ) ;
#1645 = CARTESIAN_POINT ( 'NONE',  ( -2.138189944381236884, 36.25688142232026934, -13.50000000000000000 ) ) ;
#1646 = CARTESIAN_POINT ( 'NONE',  ( 8.269754895910567782, 72.86495716742260242, -10.67059466400652212 ) ) ;
#1647 = CARTESIAN_POINT ( 'NONE',  ( 0.2546894329666128942, 79.17084467311261164, -13.49793087839145045 ) ) ;
#1648 = CARTESIAN_POINT ( 'NONE',  ( -13.49999999999999822, -15.22000000000000064, -4.386415899144240349 ) ) ;
#1649 = CARTESIAN_POINT ( 'NONE',  ( 10.92172942406179104, 60.72999999999999687, -7.935100905948385908 ) ) ;
#1650 = CARTESIAN_POINT ( 'NONE',  ( -12.66562697099517010, 53.09995439154507579, 4.693458508799205120 ) ) ;
#1651 = CARTESIAN_POINT ( 'NONE',  ( 11.76794919243112325, 40.42999999999999972, 1.441158131103945434E-15 ) ) ;
#1652 = CARTESIAN_POINT ( 'NONE',  ( 10.92172942406178926, 62.13000000000000256, 7.935100905948387684 ) ) ;
#1653 = CARTESIAN_POINT ( 'NONE',  ( -15.50189495701162379, 7.815232006635826956, -10.85006967914028131 ) ) ;
#1654 = AXIS2_PLACEMENT_3D ( 'NONE', #13119, #7658, #6418 ) ;
#1655 = CARTESIAN_POINT ( 'NONE',  ( 9.824684847845674085, 69.07009303822928814, 9.259413530656892988 ) ) ;
#1656 = CARTESIAN_POINT ( 'NONE',  ( 1.203083463835363736E-13, 37.18000000000000682, -13.50000000000000000 ) ) ;
#1657 = CARTESIAN_POINT ( 'NONE',  ( -1.844924112955495524E-14, 72.18000000000000682, -13.50000000000000000 ) ) ;
#1658 = CARTESIAN_POINT ( 'NONE',  ( -18.62500000000064659, -66.56562499999988347, 7.714727599197333419 ) ) ;
#1659 = CARTESIAN_POINT ( 'NONE',  ( -6.548632089216652297, 74.43902180796270329, 11.80836097895562808 ) ) ;
#1660 = CARTESIAN_POINT ( 'NONE',  ( -6.667109426283460927, 76.42579604055075038, -11.74159768812344851 ) ) ;
#1661 = CARTESIAN_POINT ( 'NONE',  ( 4.178864255851000829E-14, 67.68000000000000682, 13.50000000000000000 ) ) ;
#1662 = CARTESIAN_POINT ( 'NONE',  ( 19.00000000000000711, 0.000000000000000000, -1.732050807568807027 ) ) ;
#1663 = CYLINDRICAL_SURFACE ( 'NONE', #9125, 1.999999999999998224 ) ;
#1664 = CARTESIAN_POINT ( 'NONE',  ( 4.171729424061789260, 30.82999999999999474, 12.83926296998457239 ) ) ;
#1665 = CARTESIAN_POINT ( 'NONE',  ( 11.76794919243112680, -3.420000000000002593, -3.823638476888993942 ) ) ;
#1666 = EDGE_CURVE ( 'NONE', #14305, #16949, #5815, .T. ) ;
#1667 = CARTESIAN_POINT ( 'NONE',  ( 11.76794919243112325, 34.42999999999999261, 1.441158131103945434E-15 ) ) ;
#1668 = CARTESIAN_POINT ( 'NONE',  ( -8.343458848123582072, -15.62000000000000099, 11.48378591275254124 ) ) ;
#1669 = CARTESIAN_POINT ( 'NONE',  ( -8.224381812979805417, 32.36732010438169738, 10.71482383986382914 ) ) ;
#1670 = CARTESIAN_POINT ( 'NONE',  ( 13.06412971713287163, 75.55120420896997757, -3.402724263452373776 ) ) ;
#1671 = CARTESIAN_POINT ( 'NONE',  ( 3.514200034013206242, -6.916538280675000357E-15, -13.60917144867016404 ) ) ;
#1672 = CARTESIAN_POINT ( 'NONE',  ( -10.92172942406178926, 81.63000000000000966, -7.935100905948389460 ) ) ;
#1673 = DIRECTION ( 'NONE',  ( 0.000000000000000000, -1.000000000000000000, 0.000000000000000000 ) ) ;
#1674 = CARTESIAN_POINT ( 'NONE',  ( -1.563903264707652063, 38.62376394199530694, 13.40911344051972165 ) ) ;
#1675 = CARTESIAN_POINT ( 'NONE',  ( 0.06699739813339644634, 37.17759102313722508, -13.49985266111775140 ) ) ;
#1676 = CARTESIAN_POINT ( 'NONE',  ( -2.138189944381240881, 58.60311857767971588, 13.49999999999999822 ) ) ;
#1677 = CARTESIAN_POINT ( 'NONE',  ( 9.335235950531815854E-15, 58.17999999999999972, -13.50000000000000178 ) ) ;
#1678 = CARTESIAN_POINT ( 'NONE',  ( 7.724747335437769813, 62.97064110457201025, 11.07293518791896325 ) ) ;
#1679 = CARTESIAN_POINT ( 'NONE',  ( 13.49647439015347494, 42.44165888383876251, -0.3403877991304248285 ) ) ;
#1680 = CARTESIAN_POINT ( 'NONE',  ( 5.946050977868895693, 48.96319313644542603, -12.12000444874419181 ) ) ;
#1681 = CARTESIAN_POINT ( 'NONE',  ( 7.272992578804308828, 22.98000000000001108, 10.01041549318726709 ) ) ;
#1682 = ORIENTED_EDGE ( 'NONE', *, *, #4123, .T. ) ;
#1683 = CARTESIAN_POINT ( 'NONE',  ( -11.76794919243112325, 71.78000000000000114, -3.823638476888998827 ) ) ;
#1684 = CARTESIAN_POINT ( 'NONE',  ( -1.762261258681115050, 70.24333474961797208, -13.38630411701529432 ) ) ;
#1685 = CARTESIAN_POINT ( 'NONE',  ( 11.37500000000000000, -49.94999999999988205, 9.531744055041752924E-13 ) ) ;
#1686 = CARTESIAN_POINT ( 'NONE',  ( -4.171729424061791036, 5.530000000000007354, 12.83926296998457239 ) ) ;
#1687 = VERTEX_POINT ( 'NONE', #15172 ) ;
#1688 = ADVANCED_FACE ( 'NONE', ( #3072 ), #1751, .T. ) ;
#1689 = CARTESIAN_POINT ( 'NONE',  ( -11.10596490569379746, 43.64093710854871233, -7.675131488725745577 ) ) ;
#1690 = CARTESIAN_POINT ( 'NONE',  ( -7.499999999999999112, 102.9300000000000068, 9.367496997597601904 ) ) ;
#1691 = CARTESIAN_POINT ( 'NONE',  ( 7.888673446950843271, 60.88244582797990034, -10.96439275093654331 ) ) ;
#1692 = CARTESIAN_POINT ( 'NONE',  ( 2.621994543952811015E-15, 2.179999999999994831, -14.19474002721660355 ) ) ;
#1693 = LINE ( 'NONE', #11253, #4859 ) ;
#1694 = CARTESIAN_POINT ( 'NONE',  ( 10.20567559529917467, 66.09011338957789405, 8.837093107525932467 ) ) ;
#1695 = CARTESIAN_POINT ( 'NONE',  ( 3.272928082058740973, 56.79766793957027460, 13.09725250748105019 ) ) ;
#1696 = CARTESIAN_POINT ( 'NONE',  ( -3.636496289402153081, 59.32999999999999829, -11.19198476289190936 ) ) ;
#1697 = CARTESIAN_POINT ( 'NONE',  ( 13.50000000000000000, 35.42999999999999972, 1.653273178848926867E-15 ) ) ;
#1698 = CARTESIAN_POINT ( 'NONE',  ( -7.272992578804307939, 62.47999999999998977, -10.01041549318726886 ) ) ;
#1699 = CARTESIAN_POINT ( 'NONE',  ( -12.88439216619325656, 46.78478293884005978, -4.045317359391656709 ) ) ;
#1700 = CARTESIAN_POINT ( 'NONE',  ( 10.60034612014990785, 45.74832029320175764, -8.359593683353010007 ) ) ;
#1701 = CARTESIAN_POINT ( 'NONE',  ( 1.539363535742641842, 7.854661454367251494, -18.71158131929044544 ) ) ;
#1702 = SURFACE_STYLE_USAGE ( .BOTH. , #3294 ) ;
#1703 = CARTESIAN_POINT ( 'NONE',  ( 0.1761290692243684397, 31.17366705685581607, -13.49886709375031835 ) ) ;
#1704 = CARTESIAN_POINT ( 'NONE',  ( -5.514694689034828734, 56.48000644630477751, 12.32227558934507883 ) ) ;
#1705 = CARTESIAN_POINT ( 'NONE',  ( -11.37500000000039613, -42.66562499999989200, 4.711679271993002516 ) ) ;
#1706 = CARTESIAN_POINT ( 'NONE',  ( 2.445080149700053643E-15, 54.17999999999999972, -13.50000000000000000 ) ) ;
#1707 = AXIS2_PLACEMENT_3D ( 'NONE', #9878, #15401, #13115 ) ;
#1708 = CARTESIAN_POINT ( 'NONE',  ( 1.263604227248463552, 32.72543457727589100, 13.44074022279856528 ) ) ;
#1709 = CARTESIAN_POINT ( 'NONE',  ( -17.32050807568867512, 7.773118517290098062, -8.000000000000207834 ) ) ;
#1710 = ORIENTED_EDGE ( 'NONE', *, *, #6259, .F. ) ;
#1711 = ORIENTED_EDGE ( 'NONE', *, *, #5923, .T. ) ;
#1712 = CARTESIAN_POINT ( 'NONE',  ( -8.583784865206528281, 62.35052710088542227, 10.42004576716591480 ) ) ;
#1713 = VERTEX_POINT ( 'NONE', #1662 ) ;
#1714 = ADVANCED_FACE ( 'NONE', ( #8585 ), #16330, .T. ) ;
#1715 = CARTESIAN_POINT ( 'NONE',  ( -11.76794919243112325, -14.06999999999999851, -2.602085213965210642E-15 ) ) ;
#1716 = CARTESIAN_POINT ( 'NONE',  ( 13.16986379959833897, -38.46874999999992895, 13.16986379960055409 ) ) ;
#1717 = CARTESIAN_POINT ( 'NONE',  ( -12.93062576379450768, 43.79088317389158647, -3.882584947338488135 ) ) ;
#1718 = CARTESIAN_POINT ( 'NONE',  ( 8.343458848123583849, 0.8799999999999997824, -11.48378591275253768 ) ) ;
#1719 = CARTESIAN_POINT ( 'NONE',  ( -11.76794919243112325, 83.78000000000001535, -3.823638476888998827 ) ) ;
#1720 = CARTESIAN_POINT ( 'NONE',  ( -2.510641289628237960, 46.27027268115869418, -13.26455288760042173 ) ) ;
#1721 = CARTESIAN_POINT ( 'NONE',  ( -10.95561095866379908, 67.63197757295462509, -7.888270207410369217 ) ) ;
#1722 = CARTESIAN_POINT ( 'NONE',  ( 7.714727599197340524, -56.22812499999984936, 18.62500000000063949 ) ) ;
#1723 = CARTESIAN_POINT ( 'NONE',  ( 4.858184606947299145, 53.85511469388424644, 12.59567537307139951 ) ) ;
#1724 = CARTESIAN_POINT ( 'NONE',  ( -3.509521865719293032, 64.30599818513977084, -13.03769156727985745 ) ) ;
#1725 = VERTEX_POINT ( 'NONE', #9734 ) ;
#1726 = CARTESIAN_POINT ( 'NONE',  ( 15.49921147158543633, 8.062143943920768052, -9.154805866618465515 ) ) ;
#1727 = CARTESIAN_POINT ( 'NONE',  ( -8.582817366808168202, 34.50940347922665552, -10.42175089031515611 ) ) ;
#1728 = CARTESIAN_POINT ( 'NONE',  ( 4.711679271993006068, -63.47812499999984226, 11.37500000000039257 ) ) ;
#1729 = VERTEX_POINT ( 'NONE', #9648 ) ;
#1730 = CARTESIAN_POINT ( 'NONE',  ( 13.34788994058796696, 78.35896427393043950, 2.029892894008967108 ) ) ;
#1731 = CARTESIAN_POINT ( 'NONE',  ( -15.58845726811999910, 7.773118517290098950, 10.99999999999985256 ) ) ;
#1732 = CARTESIAN_POINT ( 'NONE',  ( 2.445080149700053643E-15, 36.17999999999999972, -13.50000000000000000 ) ) ;
#1733 = CARTESIAN_POINT ( 'NONE',  ( 13.47366125695251426, 72.39648660452563433, 0.9517480377630386235 ) ) ;
#1734 = CARTESIAN_POINT ( 'NONE',  ( 7.210737393588035005, 78.91145283978082148, -11.41294504455507131 ) ) ;
#1735 = CARTESIAN_POINT ( 'NONE',  ( 10.92172942406178926, -19.86999999999999744, 7.935100905948385908 ) ) ;
#1736 = CARTESIAN_POINT ( 'NONE',  ( -13.50000000000000000, 58.92999999999999972, -3.306546357697853733E-15 ) ) ;
#1737 = CARTESIAN_POINT ( 'NONE',  ( -13.13863893109200021, 52.81756508269278072, -3.169477223746528960 ) ) ;
#1738 = CARTESIAN_POINT ( 'NONE',  ( 11.76794919243112680, -18.42000000000000171, -3.823638476888993942 ) ) ;
#1739 = CARTESIAN_POINT ( 'NONE',  ( 10.92172942406179104, 56.73000000000000398, -7.935100905948385908 ) ) ;
#1740 = AXIS2_PLACEMENT_3D ( 'NONE', #9483, #6389, #3810 ) ;
#1741 = CARTESIAN_POINT ( 'NONE',  ( 0.000000000000000000, 9.000000000000000000, 0.000000000000000000 ) ) ;
#1742 = EDGE_CURVE ( 'NONE', #14262, #11444, #8498, .T. ) ;
#1743 = CARTESIAN_POINT ( 'NONE',  ( -9.520470885617715595, -5.370000000000000107, -6.917026985038136289 ) ) ;
#1744 = CARTESIAN_POINT ( 'NONE',  ( 10.91172338423278987, 69.12941896017710519, 7.948908212395449091 ) ) ;
#1745 = DIRECTION ( 'NONE',  ( 0.000000000000000000, 1.000000000000000000, 0.000000000000000000 ) ) ;
#1746 = CARTESIAN_POINT ( 'NONE',  ( -13.49999999999999822, 72.77999999999998693, -4.386415899144240349 ) ) ;
#1747 = CARTESIAN_POINT ( 'NONE',  ( 7.714727599200456254, -93.62187499999978968, -18.62499999999935341 ) ) ;
#1748 = CARTESIAN_POINT ( 'NONE',  ( -12.62315583374951800, 73.75659150799306474, -4.786044459331560752 ) ) ;
#1749 = CARTESIAN_POINT ( 'NONE',  ( -2.404533931440186567, 76.26645795944742190, -13.28413785449006035 ) ) ;
#1750 = CARTESIAN_POINT ( 'NONE',  ( -3.556480217745532916E-14, 9.046025403784437202, -12.00000000000000000 ) ) ;
#1751 = CYLINDRICAL_SURFACE ( 'NONE', #6109, 14.50000000000000000 ) ;
#1752 = CARTESIAN_POINT ( 'NONE',  ( 8.343458848123580296, 3.979999999999996430, 11.48378591275253768 ) ) ;
#1753 = CARTESIAN_POINT ( 'NONE',  ( -13.50000000000000000, 29.93000000000001393, -3.469446951953614189E-15 ) ) ;
#1754 = CARTESIAN_POINT ( 'NONE',  ( 11.76794919243112325, -9.720000000000005969, 3.823638476888996163 ) ) ;
#1755 = CARTESIAN_POINT ( 'NONE',  ( -11.76794919243112325, 39.07999999999999119, 3.823638476888994830 ) ) ;
#1756 = CARTESIAN_POINT ( 'NONE',  ( 12.00000000000000355, 5.713974596215566137, -3.899036354794874093 ) ) ;
#1757 = VECTOR ( 'NONE', #6026, 1000.000000000000000 ) ;
#1758 = CARTESIAN_POINT ( 'NONE',  ( -9.417534539751688527, 32.31048376298131330, 9.672654054616247166 ) ) ;
#1759 = CARTESIAN_POINT ( 'NONE',  ( 13.09947432517387433, 75.54609923471080890, -3.264907772012195508 ) ) ;
#1760 = CARTESIAN_POINT ( 'NONE',  ( 7.126290347628621902, 3.911145512478425917E-16, -15.45937452924531286 ) ) ;
#1761 = CARTESIAN_POINT ( 'NONE',  ( 11.76794919243112325, 31.42999999999999972, 1.441158131103945434E-15 ) ) ;
#1762 = CARTESIAN_POINT ( 'NONE',  ( 8.323493681088855567, 51.86260169611556847, -10.63262715383440415 ) ) ;
#1763 = EDGE_CURVE ( 'NONE', #1210, #13044, #4062, .T. ) ;
#1764 = CARTESIAN_POINT ( 'NONE',  ( -3.350167926867789969, 38.55967038338359032, 13.08738360368760567 ) ) ;
#1765 = CARTESIAN_POINT ( 'NONE',  ( 5.881545760074193829, 36.96579597873309098, -12.15211109713918169 ) ) ;
#1766 = DIRECTION ( 'NONE',  ( 0.000000000000000000, 1.000000000000000000, 0.000000000000000000 ) ) ;
#1767 = CARTESIAN_POINT ( 'NONE',  ( -0.7119081483307314606, 49.20556749876198666, -13.48189764473124974 ) ) ;
#1768 = CARTESIAN_POINT ( 'NONE',  ( 9.615195027071965939, 63.05942374218840030, 9.476182696171701281 ) ) ;
#1769 = CARTESIAN_POINT ( 'NONE',  ( 13.48083382501841676, 42.40518313085501489, 0.7192385255011690681 ) ) ;
#1770 = CARTESIAN_POINT ( 'NONE',  ( 9.370505335838927863, 48.81306206236823897, -9.728736506576064258 ) ) ;
#1771 = CARTESIAN_POINT ( 'NONE',  ( 11.76794919243112325, 20.28000000000000824, 3.823638476888996163 ) ) ;
#1772 = VERTEX_POINT ( 'NONE', #11050 ) ;
#1773 = CARTESIAN_POINT ( 'NONE',  ( -11.76794919243112325, 65.78000000000000114, -3.823638476888998827 ) ) ;
#1774 = CARTESIAN_POINT ( 'NONE',  ( -3.982813593950979669, 70.32320728644485541, -12.89911927572956252 ) ) ;
#1775 = CARTESIAN_POINT ( 'NONE',  ( -8.043339635996302306, -72.84374999999981526, -8.043339635997654113 ) ) ;
#1776 = CARTESIAN_POINT ( 'NONE',  ( 8.343458848123578520, 5.980000000000005755, 11.48378591275254124 ) ) ;
#1777 = ORIENTED_EDGE ( 'NONE', *, *, #8596, .F. ) ;
#1778 = CARTESIAN_POINT ( 'NONE',  ( -7.500000000000000000, 103.4443346693207957, -9.346209313438659905 ) ) ;
#1779 = CARTESIAN_POINT ( 'NONE',  ( 8.343458848123578520, 3.979999999999996430, 11.48378591275254124 ) ) ;
#1780 = CARTESIAN_POINT ( 'NONE',  ( 1.469576158976823947E-15, 108.9300000000000068, 12.00000000000000178 ) ) ;
#1781 = CARTESIAN_POINT ( 'NONE',  ( 12.02417248861142340, 66.20348976307651867, 6.144749074482731999 ) ) ;
#1782 = CARTESIAN_POINT ( 'NONE',  ( 4.951365981876046263, 56.85859764264212401, 12.55922057576340833 ) ) ;
#1783 = CARTESIAN_POINT ( 'NONE',  ( -7.272992578804310604, 60.37999999999998835, 10.01041549318726709 ) ) ;
#1784 = CARTESIAN_POINT ( 'NONE',  ( -11.76794919243112325, 68.93000000000000682, -2.882316262207890869E-15 ) ) ;
#1785 = CARTESIAN_POINT ( 'NONE',  ( -13.48997199921942780, 46.94790804180549770, 0.5203843874578459872 ) ) ;
#1786 = CARTESIAN_POINT ( 'NONE',  ( 9.145645418827751172, 45.82382894212507551, -9.930115241637599510 ) ) ;
#1787 = CARTESIAN_POINT ( 'NONE',  ( 1.760363844716795079, 70.11686978712239693, -13.39198461572166110 ) ) ;
#1788 = EDGE_CURVE ( 'NONE', #3997, #4566, #5670, .T. ) ;
#1789 = CARTESIAN_POINT ( 'NONE',  ( 5.939077118726382665, 30.96351101756093982, -12.12376556905278058 ) ) ;
#1790 = CARTESIAN_POINT ( 'NONE',  ( -8.628727929195679991, 56.34842528014506513, 10.38244214053023384 ) ) ;
#1791 = CARTESIAN_POINT ( 'NONE',  ( 10.92172942406179104, 53.72999999999999687, -7.935100905948385908 ) ) ;
#1792 = CARTESIAN_POINT ( 'NONE',  ( 4.453605494073674009, 32.84020350842553171, 12.74473092711098943 ) ) ;
#1793 = CARTESIAN_POINT ( 'NONE',  ( -6.987110303422327640, 10.00000000000000000, 10.35626373279682788 ) ) ;
#1794 = CARTESIAN_POINT ( 'NONE',  ( 4.336380559087108288, 40.02405505865456803, -12.78459519145104828 ) ) ;
#1795 = CARTESIAN_POINT ( 'NONE',  ( -8.847428061141151545, 62.33815899834955587, 10.19748488632688854 ) ) ;
#1796 = VERTEX_POINT ( 'NONE', #1830 ) ;
#1797 = CARTESIAN_POINT ( 'NONE',  ( -13.48607429853445439, 40.95120110529397550, 0.6154623111518494616 ) ) ;
#1798 = CARTESIAN_POINT ( 'NONE',  ( -18.62500000000000000, -65.52499999999986358, -1.562973063126292757E-12 ) ) ;
#1799 = CARTESIAN_POINT ( 'NONE',  ( -10.92836780634199023, 44.22976925262064896, 7.928318132319670752 ) ) ;
#1800 = CARTESIAN_POINT ( 'NONE',  ( -8.457499700851188962, 8.027799080943070820, 16.03540712409199642 ) ) ;
#1801 = CARTESIAN_POINT ( 'NONE',  ( 2.607531440858944223E-15, 34.17999999999999972, -14.19474002721660355 ) ) ;
#1802 = CARTESIAN_POINT ( 'NONE',  ( -9.615460584619185624, 46.55943716852689818, -9.475913135533545528 ) ) ;
#1803 = CARTESIAN_POINT ( 'NONE',  ( -3.396000859129791216, 67.30175415131174077, -13.06908703928144533 ) ) ;
#1804 = CARTESIAN_POINT ( 'NONE',  ( 8.043339635997652337, 5.168750000000006395, -8.043339635996304082 ) ) ;
#1805 = CARTESIAN_POINT ( 'NONE',  ( 10.64234380851644524, 54.11403152435825348, 8.306118739732548661 ) ) ;
#1806 = ORIENTED_EDGE ( 'NONE', *, *, #1955, .T. ) ;
#1807 = CARTESIAN_POINT ( 'NONE',  ( -9.211117710370606559, 64.53893790892921345, -9.889622180093912363 ) ) ;
#1808 = ORIENTED_EDGE ( 'NONE', *, *, #10473, .F. ) ;
#1809 = CARTESIAN_POINT ( 'NONE',  ( 16.47733079524782340, 7.956441929884684683, -8.178053476330095606 ) ) ;
#1810 = CARTESIAN_POINT ( 'NONE',  ( -4.131518063981246769, 34.32854624200039950, -12.85268223519957687 ) ) ;
#1811 = CARTESIAN_POINT ( 'NONE',  ( 11.37499999999960210, -48.90937499999989058, 4.711679271994918317 ) ) ;
#1812 = CARTESIAN_POINT ( 'NONE',  ( 10.56254081286317614, 78.10946437613924331, 8.407613947475192973 ) ) ;
#1813 = DIRECTION ( 'NONE',  ( -0.000000000000000000, -1.000000000000000000, -0.000000000000000000 ) ) ;
#1814 = CARTESIAN_POINT ( 'NONE',  ( 7.500000000000001776, -23.99662210092440517, 8.932545650451684693 ) ) ;
#1815 = CARTESIAN_POINT ( 'NONE',  ( 13.14030536245351222, 72.54035111403283054, -3.109320234174559161 ) ) ;
#1816 = CARTESIAN_POINT ( 'NONE',  ( 3.636496289402157078, 27.02999999999999758, -11.19198476289190936 ) ) ;
#1817 = CARTESIAN_POINT ( 'NONE',  ( 8.343458848123583849, 60.88000000000000256, -11.48378591275253768 ) ) ;
#1818 = CARTESIAN_POINT ( 'NONE',  ( -2.407714511490748777, 52.26657253894821054, -13.28356114519097808 ) ) ;
#1819 = CARTESIAN_POINT ( 'NONE',  ( -9.520470885617717371, 42.22999999999999687, 6.917026985038133624 ) ) ;
#1820 = CARTESIAN_POINT ( 'NONE',  ( -8.343458848123582072, 61.38000000000000256, 11.48378591275254124 ) ) ;
#1821 = CARTESIAN_POINT ( 'NONE',  ( -8.891200544363830713E-16, 8.679999999999999716, 13.49999999999999822 ) ) ;
#1822 = CARTESIAN_POINT ( 'NONE',  ( -9.520470885617715595, -2.369999999999996998, -6.917026985038136289 ) ) ;
#1823 = CARTESIAN_POINT ( 'NONE',  ( 7.856379207180958169, 68.97648971074549706, 10.97942687797863748 ) ) ;
#1824 = CARTESIAN_POINT ( 'NONE',  ( 0.000000000000000000, 80.93000000000000682, -13.50000000000000000 ) ) ;
#1825 = CARTESIAN_POINT ( 'NONE',  ( -13.49999999999999822, 79.07999999999999829, 4.386415899144235020 ) ) ;
#1826 = CARTESIAN_POINT ( 'NONE',  ( 18.62499999999935341, -89.45937499999983800, 7.714727599200469577 ) ) ;
#1827 = CARTESIAN_POINT ( 'NONE',  ( -13.35165232598691709, 73.86010075147470388, -1.995846695151413330 ) ) ;
#1828 = CARTESIAN_POINT ( 'NONE',  ( -7.122883083305794116, 76.44482685471382410, -11.46806178800632203 ) ) ;
#1829 = CARTESIAN_POINT ( 'NONE',  ( 0.000000000000000000, 80.93000000000000682, -13.50000000000000000 ) ) ;
#1830 = CARTESIAN_POINT ( 'NONE',  ( -5.441113646577473872, 0.000000000000000000, -25.42428528562855305 ) ) ;
#1831 = CARTESIAN_POINT ( 'NONE',  ( -10.92172942406179104, 3.230000000000010640, 7.935100905948385908 ) ) ;
#1832 = CARTESIAN_POINT ( 'NONE',  ( 10.92172942406179104, 28.73000000000000398, -7.935100905948385908 ) ) ;
#1833 = CARTESIAN_POINT ( 'NONE',  ( 7.272992578804308828, -4.019999999999998685, 10.01041549318726709 ) ) ;
#1834 = CARTESIAN_POINT ( 'NONE',  ( -7.272992578804307939, 38.47999999999999687, -10.01041549318727064 ) ) ;
#1835 = ADVANCED_BREP_SHAPE_REPRESENTATION ( '', ( #3043, #16654 ), #13005 ) ;
#1836 = UNCERTAINTY_MEASURE_WITH_UNIT (LENGTH_MEASURE( 1.000000000000000082E-05 ), #4602, 'distance_accuracy_value', 'NONE');
#1837 = CARTESIAN_POINT ( 'NONE',  ( 3.708203932499371192, 6.163974596215569868, -11.41267819554184548 ) ) ;
#1838 = CARTESIAN_POINT ( 'NONE',  ( -6.956384866273832124, 32.42216814373086464, 11.56991202652051420 ) ) ;
#1839 = CARTESIAN_POINT ( 'NONE',  ( -17.32050807568867512, 7.773118517290098062, -8.000000000000207834 ) ) ;
#1840 = EDGE_CURVE ( 'NONE', #3933, #9499, #5487, .T. ) ;
#1841 = FACE_OUTER_BOUND ( 'NONE', #9495, .T. ) ;
#1842 =( NAMED_UNIT ( * ) SI_UNIT ( $, .STERADIAN. ) SOLID_ANGLE_UNIT ( ) );
#1843 = CARTESIAN_POINT ( 'NONE',  ( 13.49999999999999822, 83.28000000000001535, 4.386415899144237684 ) ) ;
#1844 = CARTESIAN_POINT ( 'NONE',  ( 7.503935912028310007, 51.89890203572196725, -11.22317663737363702 ) ) ;
#1845 = COLOUR_RGB ( '',0.7921568627450980005, 0.8196078431372548767, 0.9333333333333333481 ) ;
#1846 = CARTESIAN_POINT ( 'NONE',  ( -4.382597213356913102, 38.52237731888514105, 12.76882425985456315 ) ) ;
#1847 = CARTESIAN_POINT ( 'NONE',  ( 1.101915621515684673, 37.14046543417862267, -13.45675805337361020 ) ) ;
#1848 = CARTESIAN_POINT ( 'NONE',  ( 25.42428528562856727, 5.918584287042170544, -5.441113646577394825 ) ) ;
#1849 = CARTESIAN_POINT ( 'NONE',  ( -0.003440076053688929415, 49.18012369244059556, -13.50000000096518171 ) ) ;
#1850 = CARTESIAN_POINT ( 'NONE',  ( 7.090050658895051150, 62.94344369233374437, 11.48830835003065687 ) ) ;
#1851 = LINE ( 'NONE', #16705, #8572 ) ;
#1852 = CARTESIAN_POINT ( 'NONE',  ( 12.30163302192313957, 48.63347965893699865, -5.560926583519345989 ) ) ;
#1853 = CARTESIAN_POINT ( 'NONE',  ( 3.636496289402154414, 25.83000000000001961, 11.19198476289190758 ) ) ;
#1854 = ORIENTED_EDGE ( 'NONE', *, *, #7375, .T. ) ;
#1855 = CARTESIAN_POINT ( 'NONE',  ( 3.636496289402157078, 68.03000000000000114, -11.19198476289190936 ) ) ;
#1856 = CARTESIAN_POINT ( 'NONE',  ( -11.37500000000039790, -18.76562499999993605, 4.711679271993001628 ) ) ;
#1857 = CARTESIAN_POINT ( 'NONE',  ( 8.043339635997654113, -85.33124999999978400, -8.043339635996304082 ) ) ;
#1858 = ORIENTED_EDGE ( 'NONE', *, *, #1666, .F. ) ;
#1859 = CARTESIAN_POINT ( 'NONE',  ( -0.6361984379052563199, 43.20287484601561800, -13.48515643269810482 ) ) ;
#1860 = CARTESIAN_POINT ( 'NONE',  ( 6.616676866212972294E-07, 41.68001839382905160, 13.49999999999996625 ) ) ;
#1861 = CIRCLE ( 'NONE', #6680, 6.000000000000001776 ) ;
#1862 = CARTESIAN_POINT ( 'NONE',  ( -10.92172942406179104, 3.230000000000010640, 7.935100905948385908 ) ) ;
#1863 = CARTESIAN_POINT ( 'NONE',  ( 18.62500000000064304, -17.69062499999995808, -7.714727599197334307 ) ) ;
#1864 = CARTESIAN_POINT ( 'NONE',  ( 10.19862847849394605, 66.08974497899659184, 8.845225045481868165 ) ) ;
#1865 = CARTESIAN_POINT ( 'NONE',  ( 8.343458848123583849, 81.87999999999999545, -11.48378591275253768 ) ) ;
#1866 = CARTESIAN_POINT ( 'NONE',  ( 11.76794919243112325, 61.42999999999999972, 1.441158131103945434E-15 ) ) ;
#1867 = CARTESIAN_POINT ( 'NONE',  ( -3.636496289402155746, 60.53000000000000114, 11.19198476289190936 ) ) ;
#1868 = CARTESIAN_POINT ( 'NONE',  ( -11.31655382394981402, 46.65401601797371001, -7.361090251168096010 ) ) ;
#1869 = CARTESIAN_POINT ( 'NONE',  ( 10.61521234890549437, 45.74748869403295259, -8.340708075779714292 ) ) ;
#1870 = CARTESIAN_POINT ( 'NONE',  ( 8.064323603043568767, 69.87423201233190184, -10.82667199018000659 ) ) ;
#1871 = CARTESIAN_POINT ( 'NONE',  ( 11.01673963448572735, 30.72451013036616274, -7.811118219500425397 ) ) ;
#1872 = CARTESIAN_POINT ( 'NONE',  ( -13.48103072664150659, 55.90526753793167103, -0.7160923547902818820 ) ) ;
#1873 = VECTOR ( 'NONE', #7755, 1000.000000000000000 ) ;
#1874 = CARTESIAN_POINT ( 'NONE',  ( -2.021419200856401144, 50.60735096884870643, 13.34783266993481909 ) ) ;
#1875 = CYLINDRICAL_SURFACE ( 'NONE', #10447, 13.50000000000000000 ) ;
#1876 = CARTESIAN_POINT ( 'NONE',  ( 2.096029675345698173, 10.00000000000000178, 12.94816314436808469 ) ) ;
#1877 = CARTESIAN_POINT ( 'NONE',  ( 11.60007046564512123, 39.68814104347146809, -6.930948736540742061 ) ) ;
#1878 = ORIENTED_EDGE ( 'NONE', *, *, #1885, .T. ) ;
#1879 = CARTESIAN_POINT ( 'NONE',  ( -10.54291226894605948, 62.25176954414765618, 8.434806978981946202 ) ) ;
#1880 = VERTEX_POINT ( 'NONE', #13487 ) ;
#1881 = CARTESIAN_POINT ( 'NONE',  ( 4.171729424061789260, 32.82999999999999829, 12.83926296998457239 ) ) ;
#1882 = CARTESIAN_POINT ( 'NONE',  ( 13.16986379960055409, -25.98124999999995310, -13.16986379959834430 ) ) ;
#1883 = ADVANCED_FACE ( 'NONE', ( #6789 ), #16399, .F. ) ;
#1884 = CARTESIAN_POINT ( 'NONE',  ( 9.586328625881087362, 48.05796286996289268, 9.505570431087681627 ) ) ;
#1885 = EDGE_CURVE ( 'NONE', #15852, #4556, #12330, .T. ) ;
#1886 = CARTESIAN_POINT ( 'NONE',  ( 8.343458848123583849, 65.87999999999999545, -11.48378591275253768 ) ) ;
#1887 = CARTESIAN_POINT ( 'NONE',  ( 2.607531440858944223E-15, 31.18000000000000327, -14.19474002721660355 ) ) ;
#1888 = CARTESIAN_POINT ( 'NONE',  ( -10.92172942406178926, 39.62999999999999545, -7.935100905948389460 ) ) ;
#1889 = CARTESIAN_POINT ( 'NONE',  ( -0.6981953365487996166, 46.20509056809714821, -13.48253838120680648 ) ) ;
#1890 = CARTESIAN_POINT ( 'NONE',  ( -0.1384335662044163251, 67.18497756035941393, -13.49929041167511201 ) ) ;
#1891 = CARTESIAN_POINT ( 'NONE',  ( 7.714727599197340524, -72.87812499999979821, 18.62500000000063949 ) ) ;
#1892 = CARTESIAN_POINT ( 'NONE',  ( 4.704861780774831637, 53.84940395589381268, 12.65445563452911770 ) ) ;
#1893 = ORIENTED_EDGE ( 'NONE', *, *, #4756, .F. ) ;
#1894 = LINE ( 'NONE', #7401, #7541 ) ;
#1895 = ORIENTED_EDGE ( 'NONE', *, *, #10755, .F. ) ;
#1896 = CARTESIAN_POINT ( 'NONE',  ( -5.977070597187598366, 34.39803108597568126, -12.10626348371989103 ) ) ;
#1897 = CARTESIAN_POINT ( 'NONE',  ( -11.37500000000039613, -75.96562499999980389, 4.711679271993002516 ) ) ;
#1898 = CARTESIAN_POINT ( 'NONE',  ( 10.45317117374106886, 78.10352698524791037, 8.542904918776255130 ) ) ;
#1899 = CARTESIAN_POINT ( 'NONE',  ( -7.499999999999996447, -18.00000000000000355, -9.000000000000001776 ) ) ;
#1900 = FACE_OUTER_BOUND ( 'NONE', #13899, .T. ) ;
#1901 = EDGE_CURVE ( 'NONE', #13655, #5466, #6883, .T. ) ;
#1902 = CARTESIAN_POINT ( 'NONE',  ( -4.171729424061791036, 37.53000000000000114, 12.83926296998457239 ) ) ;
#1903 = CARTESIAN_POINT ( 'NONE',  ( 11.44827556181972561, 72.16254353962827395, 7.154521231752505095 ) ) ;
#1904 = CARTESIAN_POINT ( 'NONE',  ( -7.272992578804307939, 33.47999999999999687, -10.01041549318726886 ) ) ;
#1905 = CARTESIAN_POINT ( 'NONE',  ( 13.49999999999999822, 60.28000000000000114, 4.386415899144237684 ) ) ;
#1906 = CARTESIAN_POINT ( 'NONE',  ( -5.895724195551247604, 52.39485670314912369, -12.14464293266051698 ) ) ;
#1907 = CARTESIAN_POINT ( 'NONE',  ( 9.520470885617717371, 37.72999999999999687, -6.917026985038131848 ) ) ;
#1908 = CARTESIAN_POINT ( 'NONE',  ( -9.520470885617715595, -14.37000000000000099, -6.917026985038136289 ) ) ;
#1909 = CARTESIAN_POINT ( 'NONE',  ( -13.49999999999999822, 57.77999999999999403, -4.386415899144240349 ) ) ;
#1910 = CYLINDRICAL_SURFACE ( 'NONE', #7871, 1.999999999999998224 ) ;
#1911 = CARTESIAN_POINT ( 'NONE',  ( 2.279995255611139653E-15, -5.820000000000007390, -12.37355403259654985 ) ) ;
#1912 = CARTESIAN_POINT ( 'NONE',  ( 12.49006955709644195, 69.24340693049718709, 5.129082213196267226 ) ) ;
#1913 = CARTESIAN_POINT ( 'NONE',  ( 10.92172942406179104, 71.73000000000000398, -7.935100905948385908 ) ) ;
#1914 = CARTESIAN_POINT ( 'NONE',  ( -1.564113515457998370E-12, -69.68749999999984368, 18.62500000000000000 ) ) ;
#1915 = CARTESIAN_POINT ( 'NONE',  ( -10.57228623158748526, 73.61011962570297840, -8.395047735362636487 ) ) ;
#1916 = CARTESIAN_POINT ( 'NONE',  ( -7.192128558827187490, 76.44775770338405607, -11.42468648059192837 ) ) ;
#1917 = CARTESIAN_POINT ( 'NONE',  ( -17.42428528562871293, 0.000000000000000000, 19.29752010712834220 ) ) ;
#1918 = FACE_OUTER_BOUND ( 'NONE', #7402, .T. ) ;
#1919 = CARTESIAN_POINT ( 'NONE',  ( 4.171729424061791924, 29.03000000000000114, -12.83926296998457239 ) ) ;
#1920 = CARTESIAN_POINT ( 'NONE',  ( -11.76794919243112325, -11.22000000000000242, -3.823638476888998827 ) ) ;
#1921 = CARTESIAN_POINT ( 'NONE',  ( -9.520470885617717371, 39.23000000000000398, 6.917026985038133624 ) ) ;
#1922 = CARTESIAN_POINT ( 'NONE',  ( -13.14483242576228506, 7.170662809914417402, 16.82677684650020211 ) ) ;
#1923 = EDGE_CURVE ( 'NONE', #16171, #1419, #14105, .T. ) ;
#1924 = CARTESIAN_POINT ( 'NONE',  ( -9.596645353049856553, 32.30153765603851213, 9.496518015433528248 ) ) ;
#1925 = CARTESIAN_POINT ( 'NONE',  ( 8.345963094611027699, 74.99851540925725146, 10.61115790671126824 ) ) ;
#1926 = DIRECTION ( 'NONE',  ( 0.000000000000000000, 0.000000000000000000, 1.000000000000000000 ) ) ;
#1927 = CARTESIAN_POINT ( 'NONE',  ( -13.49999999999999822, 81.77999999999998693, -4.386415899144240349 ) ) ;
#1928 = CARTESIAN_POINT ( 'NONE',  ( -2.514712666923160089, 58.27041958369694186, -13.26394781517377197 ) ) ;
#1929 =( BOUNDED_CURVE ( )  B_SPLINE_CURVE ( 2, ( #12029, #11772, #5236, #7889, #15901, #11944, #10793, #17324, #15814, #3719, #6734 ),
 .UNSPECIFIED., .F., .F. ) 
 B_SPLINE_CURVE_WITH_KNOTS ( ( 3, 2, 2, 2, 2, 3 ),
 ( 0.9583333333333333703, 0.9611111111111111382, 0.9666666666666666741, 0.9722222222222222099, 0.9777777777777777457, 0.9814746766279994761 ),
 .UNSPECIFIED. ) 
 CURVE ( )  GEOMETRIC_REPRESENTATION_ITEM ( )  RATIONAL_B_SPLINE_CURVE ( ( 0.9755282581475768211, 0.9755282581475768211, 1.000000000000000000, 0.9510565162951535312, 1.000000000000000000, 0.9510565162951535312, 1.000000000000000000, 0.9510565162951535312, 1.000000000000000000, 0.9674309604458272149, 0.9782075210486875783 ) ) 
 REPRESENTATION_ITEM ( '' )  );
#1930 = CARTESIAN_POINT ( 'NONE',  ( -6.972538664597516700, 38.42149079469095341, 11.56005070210786734 ) ) ;
#1931 = DIRECTION ( 'NONE',  ( 0.000000000000000000, -1.000000000000000000, 0.000000000000000000 ) ) ;
#1932 = DIRECTION ( 'NONE',  ( 0.000000000000000000, 0.000000000000000000, 1.000000000000000000 ) ) ;
#1933 = CARTESIAN_POINT ( 'NONE',  ( -0.03211762735042347078, 49.18115476286282473, -13.49996724290573979 ) ) ;
#1934 = CARTESIAN_POINT ( 'NONE',  ( 2.637116012700283285, 62.77482290688431021, 13.23992697210385572 ) ) ;
#1935 = CARTESIAN_POINT ( 'NONE',  ( 3.009781244587141025, 41.78827560020220488, 13.16026029025977628 ) ) ;
#1936 = CARTESIAN_POINT ( 'NONE',  ( 11.19356376271605313, 48.71361357092671085, -7.550568776909073243 ) ) ;
#1937 = CARTESIAN_POINT ( 'NONE',  ( 9.520470885617717371, 20.72999999999999687, -6.917026985038131848 ) ) ;
#1938 = ORIENTED_EDGE ( 'NONE', *, *, #15386, .T. ) ;
#1939 = CARTESIAN_POINT ( 'NONE',  ( 11.76794919243112680, 64.57999999999999829, -3.823638476888993942 ) ) ;
#1940 = CARTESIAN_POINT ( 'NONE',  ( 11.37499999999960565, -25.00937499999992397, 4.711679271994918317 ) ) ;
#1941 = CARTESIAN_POINT ( 'NONE',  ( -11.37500000000039613, -26.01562499999994316, 4.711679271993001628 ) ) ;
#1942 = CARTESIAN_POINT ( 'NONE',  ( 8.343458848123578520, 2.979999999999998650, 11.48378591275254124 ) ) ;
#1943 = CARTESIAN_POINT ( 'NONE',  ( -0.2574321900957359799, 43.18925615523563266, -13.49768559512680532 ) ) ;
#1944 = CARTESIAN_POINT ( 'NONE',  ( 0.8771553176865662937, 76.14846073976488583, -13.47147415929084246 ) ) ;
#1945 = CARTESIAN_POINT ( 'NONE',  ( -7.714727599197334307, -55.15312499999986784, -18.62500000000064304 ) ) ;
#1946 = CARTESIAN_POINT ( 'NONE',  ( 10.41011842078191485, 66.10092527843147536, 8.596008750921665609 ) ) ;
#1947 = CARTESIAN_POINT ( 'NONE',  ( 3.636496289402157078, 47.02999999999999403, -11.19198476289190936 ) ) ;
#1948 = CARTESIAN_POINT ( 'NONE',  ( -11.76794919243112325, 60.07999999999999119, 3.823638476888994386 ) ) ;
#1949 = CARTESIAN_POINT ( 'NONE',  ( -13.49209704812250088, 46.94588263088257207, 0.4618880482851102087 ) ) ;
#1950 = AXIS2_PLACEMENT_3D ( 'NONE', #2650, #9585, #14676 ) ;
#1951 = CARTESIAN_POINT ( 'NONE',  ( 11.79604064620621706, 45.67344517854842678, -6.565341261686152841 ) ) ;
#1952 = CARTESIAN_POINT ( 'NONE',  ( 5.408880282457495525, 69.98389750586773062, -12.36993325487214790 ) ) ;
#1953 =( NAMED_UNIT ( * ) PLANE_ANGLE_UNIT ( ) SI_UNIT ( $, .RADIAN. ) );
#1954 = CARTESIAN_POINT ( 'NONE',  ( 8.881221276511888973, 30.83659605439422791, -10.16962065716281849 ) ) ;
#1955 = EDGE_CURVE ( 'NONE', #17318, #16659, #12956, .T. ) ;
#1956 = CARTESIAN_POINT ( 'NONE',  ( -10.72093770326768336, 56.24171596241757953, 8.207164309218791587 ) ) ;
#1957 = CARTESIAN_POINT ( 'NONE',  ( -2.321280251217487045, 50.59645969408896349, 13.29947824124915634 ) ) ;
#1958 = DIRECTION ( 'NONE',  ( 0.000000000000000000, -1.000000000000000000, 0.000000000000000000 ) ) ;
#1959 = AXIS2_PLACEMENT_3D ( 'NONE', #10154, #3233, #8653 ) ;
#1960 = CARTESIAN_POINT ( 'NONE',  ( 5.377587941663005466, 42.98529261702660165, -12.38364086756679860 ) ) ;
#1961 = CARTESIAN_POINT ( 'NONE',  ( 10.14338171936946154, 39.77323046559094166, -8.908990778934798627 ) ) ;
#1962 = ORIENTED_EDGE ( 'NONE', *, *, #16117, .F. ) ;
#1963 = CARTESIAN_POINT ( 'NONE',  ( -12.59302166875140649, 62.10670518965311970, 4.872780399208760826 ) ) ;
#1964 = ORIENTED_EDGE ( 'NONE', *, *, #2233, .T. ) ;
#1965 = CARTESIAN_POINT ( 'NONE',  ( -13.49999999999999822, 31.78000000000000469, -4.386415899144240349 ) ) ;
#1966 = CARTESIAN_POINT ( 'NONE',  ( 7.714727599197340524, -87.37812499999982663, 18.62500000000063949 ) ) ;
#1967 = CARTESIAN_POINT ( 'NONE',  ( 12.40660301870904547, 48.23542586493246631, 5.339298433682001743 ) ) ;
#1968 = CARTESIAN_POINT ( 'NONE',  ( 4.871064484081401247, 58.00440576964228967, -12.59088220141806680 ) ) ;
#1969 = CARTESIAN_POINT ( 'NONE',  ( -9.520470885617715595, 74.62999999999999545, -6.917026985038136289 ) ) ;
#1970 = CARTESIAN_POINT ( 'NONE',  ( 10.15710352110371240, -3.110307960253506586E-15, -6.885784913371308491 ) ) ;
#1971 = CARTESIAN_POINT ( 'NONE',  ( -9.640625755184249357, 46.56070477685496201, -9.450320721539682722 ) ) ;
#1972 = EDGE_CURVE ( 'NONE', #10231, #6836, #1017, .T. ) ;
#1973 = CARTESIAN_POINT ( 'NONE',  ( -15.58845726811999910, 7.773118517290098950, 10.99999999999985256 ) ) ;
#1974 = CARTESIAN_POINT ( 'NONE',  ( 8.043339635997652337, -11.48124999999995488, -8.043339635996304082 ) ) ;
#1975 = CARTESIAN_POINT ( 'NONE',  ( 5.053712973672062070, 53.86243577901412749, 12.51843150850086950 ) ) ;
#1976 = VERTEX_POINT ( 'NONE', #6169 ) ;
#1977 = DIRECTION ( 'NONE',  ( -1.000000000000000000, -0.000000000000000000, -0.000000000000000000 ) ) ;
#1978 = ORIENTED_EDGE ( 'NONE', *, *, #1049, .F. ) ;
#1979 = LINE ( 'NONE', #4570, #6376 ) ;
#1980 = CARTESIAN_POINT ( 'NONE',  ( -6.490732267001422251, 34.41855503382694081, -11.84349393051573252 ) ) ;
#1981 = CARTESIAN_POINT ( 'NONE',  ( -11.37499999999960210, -31.18437499999994245, -4.711679271994911211 ) ) ;
#1982 = CARTESIAN_POINT ( 'NONE',  ( 10.46369314345858115, 78.10409437138895328, 8.530013921288347234 ) ) ;
#1983 = CARTESIAN_POINT ( 'NONE',  ( 16.97734196418687702, 7.854010772509913529, 8.022095340454528767 ) ) ;
#1984 = DIRECTION ( 'NONE',  ( 0.000000000000000000, 0.000000000000000000, 1.000000000000000000 ) ) ;
#1985 = CARTESIAN_POINT ( 'NONE',  ( 12.53173586800322248, 72.61303021391049128, -5.039560880771795759 ) ) ;
#1986 = CARTESIAN_POINT ( 'NONE',  ( 7.868511876303293739, 66.88295471898928213, -10.96986588721461686 ) ) ;
#1987 = CARTESIAN_POINT ( 'NONE',  ( 9.520470885617717371, 26.73000000000000398, -6.917026985038131848 ) ) ;
#1988 = CARTESIAN_POINT ( 'NONE',  ( 8.343458848123583849, 66.87999999999998124, -11.48378591275253768 ) ) ;
#1989 = CARTESIAN_POINT ( 'NONE',  ( -5.803408828651975604, 52.39120852067574674, -12.18894770220534340 ) ) ;
#1990 = CARTESIAN_POINT ( 'NONE',  ( -7.576616670048093940E-16, 36.67999999999999972, 12.37355403259654985 ) ) ;
#1991 = CARTESIAN_POINT ( 'NONE',  ( 11.76794919243112680, -15.41999999999999993, -3.823638476888993942 ) ) ;
#1992 = CARTESIAN_POINT ( 'NONE',  ( -4.171729424061787483, 54.33000000000000540, -12.83926296998457417 ) ) ;
#1993 = CARTESIAN_POINT ( 'NONE',  ( 4.171729424061789260, 76.83000000000001251, 12.83926296998457417 ) ) ;
#1994 = CARTESIAN_POINT ( 'NONE',  ( -11.76794919243112325, 0.7799999999999955858, -3.823638476888998827 ) ) ;
#1995 = CARTESIAN_POINT ( 'NONE',  ( -8.590017591600245694, 68.35022873601761262, 10.41449206865405586 ) ) ;
#1996 = CARTESIAN_POINT ( 'NONE',  ( 18.62500000000000000, -33.29999999999991900, 1.560692158462880521E-12 ) ) ;
#1997 = ADVANCED_FACE ( 'NONE', ( #12697 ), #7223, .T. ) ;
#1998 = CARTESIAN_POINT ( 'NONE',  ( 4.171729424061791924, 72.03000000000000114, -12.83926296998457239 ) ) ;
#1999 = CARTESIAN_POINT ( 'NONE',  ( 18.62500000000000000, -57.19999999999988916, 1.560692158462880521E-12 ) ) ;
#2000 = CARTESIAN_POINT ( 'NONE',  ( -13.49051361190299225, 73.91252456243813640, -0.5067315784123872513 ) ) ;
#2001 = CARTESIAN_POINT ( 'NONE',  ( -7.185958069586803276, 76.44749624477539385, -11.42856400538557438 ) ) ;
#2002 = CARTESIAN_POINT ( 'NONE',  ( 11.00000000000001599, 7.773118517290098062, -15.58845726811988364 ) ) ;
#2003 = FACE_OUTER_BOUND ( 'NONE', #13021, .T. ) ;
#2004 = CARTESIAN_POINT ( 'NONE',  ( 13.49999999999999822, 25.28000000000000824, 4.386415899144237684 ) ) ;
#2005 = CARTESIAN_POINT ( 'NONE',  ( -9.520470885617715595, 38.62999999999999545, -6.917026985038136289 ) ) ;
#2006 = CARTESIAN_POINT ( 'NONE',  ( 7.416407864998736166, 5.113974596215570045, 10.20780970022447853 ) ) ;
#2007 = CARTESIAN_POINT ( 'NONE',  ( -0.5930734014913793262, 40.20132500410929310, -13.49999994548272930 ) ) ;
#2008 = CARTESIAN_POINT ( 'NONE',  ( -7.025999278210586674, 32.41925472474766678, 11.52783640645312246 ) ) ;
#2009 = CARTESIAN_POINT ( 'NONE',  ( 8.444502319668561796, 75.00303538791125391, 10.53290446549366344 ) ) ;
#2010 = DIRECTION ( 'NONE',  ( 0.000000000000000000, -1.000000000000000000, 0.000000000000000000 ) ) ;
#2011 = CARTESIAN_POINT ( 'NONE',  ( 4.171729424061789260, 79.82999999999999829, 12.83926296998457417 ) ) ;
#2012 = CARTESIAN_POINT ( 'NONE',  ( 13.23734291971121735, 51.52354072660591555, -2.650047768604904430 ) ) ;
#2013 = CARTESIAN_POINT ( 'NONE',  ( -12.89949653176691236, 38.07337467622953397, 3.996097449710631189 ) ) ;
#2014 = EDGE_CURVE ( 'NONE', #16449, #7842, #11636, .T. ) ;
#2015 = CARTESIAN_POINT ( 'NONE',  ( 6.225595394061742560, 36.95216596563231803, -11.98154833774320593 ) ) ;
#2016 = CARTESIAN_POINT ( 'NONE',  ( 4.711679271994911211, -10.37187499999999396, -11.37499999999960210 ) ) ;
#2017 = DIRECTION ( 'NONE',  ( 0.000000000000000000, 0.000000000000000000, -1.000000000000000000 ) ) ;
#2018 = PLANE ( 'NONE',  #7825 ) ;
#2019 = VECTOR ( 'NONE', #7571, 1000.000000000000000 ) ;
#2020 = CARTESIAN_POINT ( 'NONE',  ( 0.2399344713086168090, 62.68862715799873797, 13.49787121004495205 ) ) ;
#2021 = CARTESIAN_POINT ( 'NONE',  ( -11.84443143481805549, 80.93000000000000682, 1.125603796807419066 ) ) ;
#2023 = CARTESIAN_POINT ( 'NONE',  ( 13.46220260918281575, 48.46811850303037517, -1.097924244589963738 ) ) ;
#2022 = B_SPLINE_CURVE_WITH_KNOTS ( 'NONE', 3,
 ( #14856, #8183, #9599, #13544, #6852, #8359, #4186, #14950, #297, #2840, #7197, #642, #15213, #3110, #5791, #12667, #9863, #386, #12584, #16550, #16807, #16722, #15298, #3291, #3017, #11176, #13887, #8537, #4629, #1786, #472, #3381, #5881, #11261, #14150, #16639, #4544, #6053, #9949, #3200, #4457, #12844, #10036, #1700, #1869, #8620, #8707, #15384, #13974, #14066, #8448, #7284, #559, #5966, #15470, #11347, #1951, #13802, #2039, #12500, #7376, #15119, #7114, #12753, #8792, #4714, #11435, #7463, #10117, #9773, #4364, #732, #6140, #11519, #2377, #808, #4971, #14403, #8963, #13271, #14319, #4885, #6569, #10374, #13096, #4800, #15554, #982, #8880, #14235, #16896, #7812, #6305, #10202, #2120, #1159, #15820, #3466, #13185, #7546, #1070, #6395, #12924, #15728, #6220, #2207, #3636, #9228, #9050, #11606, #16982, #5153, #10287, #15639, #3549, #7634, #13012, #2291, #892, #10460, #14582, #11690, #17067, #7720, #6483, #11778, #17154, #5065, #3725, #9143, #14490, #11868, #7894, #17243, #10546, #15906, #3815, #2463, #16345, #97, #10713, #9661, #8334, #4252, #12294, #14833, #10886, #9401, #13607, #6, #10975, #7982, #16255, #14750, #1502, #5411, #15011, #13351, #5328, #12204, #3985, #9574, #10627, #5241, #15992, #13520, #6917, #3896, #17413, #9314, #2902, #13689, #1589, #6826, #14664 ),
 .UNSPECIFIED., .F., .F.,
 ( 4, 2, 1, 1, 1, 2, 2, 1, 2, 2, 2, 2, 2, 2, 2, 2, 2, 1, 2, 2, 1, 1, 1, 2, 2, 1, 2, 2, 2, 2, 2, 2, 2, 2, 2, 2, 2, 2, 1, 1, 2, 2, 2, 2, 1, 2, 2, 1, 1, 2, 2, 2, 2, 2, 2, 2, 2, 2, 2, 2, 1, 2, 2, 1, 1, 1, 1, 1, 1, 2, 2, 1, 2, 2, 2, 2, 1, 1, 1, 2, 2, 1, 1, 1, 2, 2, 2, 2, 1, 2, 2, 1, 1, 2, 2, 2, 2, 2, 2, 1, 1, 2, 2, 4 ),
 ( 0.6813842983133263642, 0.6850787074223488871, 0.6853096079916627392, 0.6853384705628270401, 0.6853529018484091351, 0.6853601174912001825, 0.6853673331339912300, 0.6854250582763197208, 0.6855405085609765914, 0.6860023096996044067, 0.6864641108382321111, 0.6866950114075460743, 0.6868104616922029448, 0.6868681868345314356, 0.6869259119768599264, 0.6878495142541154461, 0.6883113153927431505, 0.6883401779639074514, 0.6883473936066984988, 0.6883546092494895463, 0.6883690405350716413, 0.6884267656774001320, 0.6885422159620571136, 0.6887731165313710768, 0.6896967188086268186, 0.6898121690932838002, 0.6898410316644479900, 0.6898698942356122910, 0.6899276193779407818, 0.6901585199472547449, 0.6906203210858826713, 0.6910821222245104867, 0.6913130227938244499, 0.6914284730784814315, 0.6915439233631384131, 0.6924675256403942658, 0.6933911279176502296, 0.6936220284869641928, 0.6937374787716211744, 0.6937952039139496652, 0.6938240664851138551, 0.6938529290562781560, 0.6943147301949060823, 0.6961619347494177878, 0.6962773850340747694, 0.6963062476052389593, 0.6963206788908211653, 0.6963351101764032602, 0.6963928353187317510, 0.6966237358880457142, 0.6970855370266736406, 0.6980091393039293823, 0.6984709404425573087, 0.6987018410118712719, 0.6987595661541997627, 0.6988172912965282535, 0.6989327415811852351, 0.6998563438584410878, 0.7007799461356968296, 0.7012417472743247560, 0.7012706098454890569, 0.7012850411310711518, 0.7012994724166532468, 0.7013571975589817376, 0.7014726478436387191, 0.7017035484129525713, 0.7021653495515804977, 0.7023962501208944609, 0.7025117004055514425, 0.7025405629767156324, 0.7025549942622977273, 0.7025694255478798222, 0.7026271506902083130, 0.7035507529674639438, 0.7037816535367779069, 0.7038105161079420968, 0.7038393786791063977, 0.7038971038214348885, 0.7040125541060918701, 0.7044743552447196855, 0.7053979575219755382, 0.7058597586606033536, 0.7060906592299173168, 0.7062061095145742984, 0.7062638346569027892, 0.7063215597992312800, 0.7072451620764870217, 0.7074760626458009849, 0.7075049252169652858, 0.7075193565025473807, 0.7075265721453384282, 0.7075337877881294757, 0.7075915129304579665, 0.7077069632151149481, 0.7081687643537428745, 0.7086305654923708008, 0.7087460157770278935, 0.7087604470626099884, 0.7087748783481920833, 0.7088037409193563843, 0.7088614660616848751, 0.7090923666309989493, 0.7100159689082550241, 0.7109395711855112099 ),
 .UNSPECIFIED. ) ;
#2024 = CARTESIAN_POINT ( 'NONE',  ( -9.520470885617715595, 21.63000000000000966, -6.917026985038136289 ) ) ;
#2025 = ORIENTED_EDGE ( 'NONE', *, *, #5375, .F. ) ;
#2026 = CARTESIAN_POINT ( 'NONE',  ( -11.76794919243112325, 63.07999999999999829, 3.823638476888994830 ) ) ;
#2027 = CARTESIAN_POINT ( 'NONE',  ( 11.37500000000000178, -9.399999999999959499, 9.531744055041752924E-13 ) ) ;
#2028 = CARTESIAN_POINT ( 'NONE',  ( -8.043339635997654113, -27.05624999999993463, 8.043339635996302306 ) ) ;
#2029 = CARTESIAN_POINT ( 'NONE',  ( 2.621994543952811015E-15, 1.180000000000004601, -14.19474002721660355 ) ) ;
#2030 = CARTESIAN_POINT ( 'NONE',  ( 7.272992578804308828, 31.98000000000000043, 10.01041549318726709 ) ) ;
#2031 = CARTESIAN_POINT ( 'NONE',  ( -8.000000000000143885, 7.773118517290097174, 17.32050807568870709 ) ) ;
#2032 = CARTESIAN_POINT ( 'NONE',  ( 13.16986379959834075, -47.86874999999988489, 13.16986379960055231 ) ) ;
#2033 = CARTESIAN_POINT ( 'NONE',  ( 12.47450349530925351, 66.24198063057153263, 5.166296410220359903 ) ) ;
#2034 = CARTESIAN_POINT ( 'NONE',  ( 6.750022565184456980, 31.92926174983938026, 11.69132992304556495 ) ) ;
#2035 = CARTESIAN_POINT ( 'NONE',  ( -9.520470885617715595, 50.62999999999999545, -6.917026985038136289 ) ) ;
#2036 = CARTESIAN_POINT ( 'NONE',  ( 8.343458848123583849, 7.880000000000003446, -11.48378591275253768 ) ) ;
#2037 = VECTOR ( 'NONE', #11526, 1000.000000000000000 ) ;
#2038 = CARTESIAN_POINT ( 'NONE',  ( -9.949452233774618293, 59.28342264085854652, 9.124606215017720956 ) ) ;
#2039 = CARTESIAN_POINT ( 'NONE',  ( 11.81973372649256149, 45.67171577755837575, -6.522591581979077624 ) ) ;
#2040 = CARTESIAN_POINT ( 'NONE',  ( 9.936708544982330693, 69.78412393671250413, -9.139967157036311463 ) ) ;
#2041 = CARTESIAN_POINT ( 'NONE',  ( -11.52888015854957793, 80.93000000000003524, 3.329402692645399675 ) ) ;
#2042 = CARTESIAN_POINT ( 'NONE',  ( 12.02698711349998817, 30.65606005353055963, -6.132014165155652563 ) ) ;
#2043 = CARTESIAN_POINT ( 'NONE',  ( -13.45917019767884426, 55.96633912471227745, 1.049381195819143242 ) ) ;
#2044 = CARTESIAN_POINT ( 'NONE',  ( -3.622045108825971305, 50.54975662805617986, 13.00518533329681148 ) ) ;
#2045 = CARTESIAN_POINT ( 'NONE',  ( 13.29382772739631058, 33.34733514712192459, 2.350360117349177713 ) ) ;
#2046 = CARTESIAN_POINT ( 'NONE',  ( 0.6483769335424683922, 43.15676486429432401, -13.48533567729083416 ) ) ;
#2047 = CARTESIAN_POINT ( 'NONE',  ( 11.20965635938246585, 39.71270877404705146, -7.522876792059077999 ) ) ;
#2048 = EDGE_LOOP ( 'NONE', ( #10560, #17210, #15194, #3651, #15479 ) ) ;
#2049 = CARTESIAN_POINT ( 'NONE',  ( -13.46752786525881795, 61.89760212117944604, -0.9386075886148094183 ) ) ;
#2050 = VERTEX_POINT ( 'NONE', #14002 ) ;
#2051 = AXIS2_PLACEMENT_3D ( 'NONE', #7764, #8829, #13136 ) ;
#2052 = ORIENTED_EDGE ( 'NONE', *, *, #12150, .T. ) ;
#2053 = CARTESIAN_POINT ( 'NONE',  ( 9.520470885617717371, -18.27000000000000313, -6.917026985038131848 ) ) ;
#2054 = CARTESIAN_POINT ( 'NONE',  ( 13.16986379959833897, -105.0687499999997527, 13.16986379960055409 ) ) ;
#2055 = CARTESIAN_POINT ( 'NONE',  ( 4.737298224311091488, 58.00936883926053866, -12.64152061320751663 ) ) ;
#2056 = CARTESIAN_POINT ( 'NONE',  ( 7.310637651931115144, 78.90721144323025271, -11.34975570436828285 ) ) ;
#2057 = EDGE_CURVE ( 'NONE', #3274, #106, #1979, .T. ) ;
#2058 = CARTESIAN_POINT ( 'NONE',  ( 3.636496289402154414, 78.82999999999999829, 11.19198476289190936 ) ) ;
#2059 = CARTESIAN_POINT ( 'NONE',  ( -13.50000000000000000, 42.92999999999999261, -3.306546357697853733E-15 ) ) ;
#2060 = CARTESIAN_POINT ( 'NONE',  ( 10.59082145838073075, -1.242015572811692772E-15, 8.046083559367682270 ) ) ;
#2061 = CARTESIAN_POINT ( 'NONE',  ( 11.37500000000039613, -27.09062499999992113, -4.711679271993004292 ) ) ;
#2062 = CARTESIAN_POINT ( 'NONE',  ( 7.041864955729037590, 53.94154545869297834, 11.52006337894699861 ) ) ;
#2063 = CARTESIAN_POINT ( 'NONE',  ( 11.76794919243112680, 14.57999999999999474, -3.823638476888993942 ) ) ;
#2064 = ORIENTED_EDGE ( 'NONE', *, *, #15044, .F. ) ;
#2065 = LINE ( 'NONE', #7666, #1873 ) ;
#2066 = ORIENTED_EDGE ( 'NONE', *, *, #2974, .F. ) ;
#2067 = CARTESIAN_POINT ( 'NONE',  ( 6.299111959984896814, 66.94929370039956495, -11.94646788586564057 ) ) ;
#2068 = CARTESIAN_POINT ( 'NONE',  ( -11.37500000000039613, -92.61562499999978115, 4.711679271993002516 ) ) ;
#2069 = CARTESIAN_POINT ( 'NONE',  ( 1.553912808195373474, 77.73587740583015204, 13.41073184109523453 ) ) ;
#2070 = FACE_OUTER_BOUND ( 'NONE', #2391, .T. ) ;
#2071 = CARTESIAN_POINT ( 'NONE',  ( 17.32050807568878170, 7.773118517290099838, -7.999999999999961808 ) ) ;
#2072 = CYLINDRICAL_SURFACE ( 'NONE', #9913, 1.999999999999998224 ) ;
#2073 = CARTESIAN_POINT ( 'NONE',  ( 12.18022657597662040, 72.21555684226325411, 5.843038593813369097 ) ) ;
#2074 = CARTESIAN_POINT ( 'NONE',  ( -7.272992578804310604, 31.38000000000002032, 10.01041549318726709 ) ) ;
#2075 = CARTESIAN_POINT ( 'NONE',  ( -4.171729424061787483, 49.32999999999999829, -12.83926296998457417 ) ) ;
#2076 = CARTESIAN_POINT ( 'NONE',  ( -0.3661892661420289574, 71.66683318614190057, 13.49503404522676853 ) ) ;
#2077 = CARTESIAN_POINT ( 'NONE',  ( -4.171729424061787483, 51.32999999999999829, -12.83926296998457417 ) ) ;
#2078 = CARTESIAN_POINT ( 'NONE',  ( 18.18340077413957090, 8.007813497946154158, 0.8546369493909243831 ) ) ;
#2079 = CARTESIAN_POINT ( 'NONE',  ( -10.72979123883553676, 68.24212118105015179, 8.239908094999801591 ) ) ;
#2080 = CARTESIAN_POINT ( 'NONE',  ( 18.62499999999934630, -15.60937499999996270, 7.714727599200467800 ) ) ;
#2081 = CARTESIAN_POINT ( 'NONE',  ( 2.138189944381238661, 70.75688142232027644, 13.50000000000000000 ) ) ;
#2082 = CARTESIAN_POINT ( 'NONE',  ( 18.62500000000064304, -50.99062499999987352, -7.714727599197335195 ) ) ;
#2083 = CARTESIAN_POINT ( 'NONE',  ( -2.522042593689474810, 65.58931665179493109, 13.26232815706891266 ) ) ;
#2084 = CYLINDRICAL_SURFACE ( 'NONE', #12693, 12.00000000000000178 ) ;
#2085 = CARTESIAN_POINT ( 'NONE',  ( 8.099236140987171595, 7.915750619362869500, -16.68483048229433763 ) ) ;
#2086 = ORIENTED_EDGE ( 'NONE', *, *, #16024, .F. ) ;
#2087 = FACE_OUTER_BOUND ( 'NONE', #4655, .T. ) ;
#2088 = DIRECTION ( 'NONE',  ( 0.000000000000000000, 0.000000000000000000, -1.000000000000000000 ) ) ;
#2089 = CARTESIAN_POINT ( 'NONE',  ( -3.476970977993532941, 40.30499584707952465, -13.04628310429154148 ) ) ;
#2090 = CARTESIAN_POINT ( 'NONE',  ( -12.92717612063876587, 31.79057794579883023, -3.890979012274611737 ) ) ;
#2091 = CARTESIAN_POINT ( 'NONE',  ( 5.607300059319721974, 74.88362207002212756, 12.28117982223269600 ) ) ;
#2092 = EDGE_CURVE ( 'NONE', #13131, #5168, #14123, .T. ) ;
#2093 = CARTESIAN_POINT ( 'NONE',  ( -18.99999999999998224, 0.000000000000000000, -1.732050807569074369 ) ) ;
#2094 = DIRECTION ( 'NONE',  ( -0.8520478343185368120, -2.529072625723438252E-21, -0.5234639319314094985 ) ) ;
#2095 = CARTESIAN_POINT ( 'NONE',  ( 2.607531440858944223E-15, 72.18000000000000682, -14.19474002721660355 ) ) ;
#2096 = CARTESIAN_POINT ( 'NONE',  ( 12.64609271680043179, 51.60106898862535019, -4.725079458178631064 ) ) ;
#2097 = CARTESIAN_POINT ( 'NONE',  ( -13.48282497468361818, 37.90642807506478107, -0.6813083995204127774 ) ) ;
#2098 = CARTESIAN_POINT ( 'NONE',  ( 12.02800223548316616, 36.65598124211443576, -6.130211025472831921 ) ) ;
#2099 = CARTESIAN_POINT ( 'NONE',  ( -8.043339635997652337, -50.95624999999989768, 8.043339635996300530 ) ) ;
#2100 = CARTESIAN_POINT ( 'NONE',  ( 2.222800136090958073E-15, 3.046025403784441643, -12.00000000000000000 ) ) ;
#2101 = CARTESIAN_POINT ( 'NONE',  ( -0.8913732225149532118, 77.64795571117363693, 13.47771292552425670 ) ) ;
#2102 = DIRECTION ( 'NONE',  ( 0.000000000000000000, -1.000000000000000000, 0.000000000000000000 ) ) ;
#2103 = FACE_OUTER_BOUND ( 'NONE', #1466, .T. ) ;
#2104 = CARTESIAN_POINT ( 'NONE',  ( 13.50015753368874094, 48.42919927454262563, 0.02489017590083256182 ) ) ;
#2105 = CARTESIAN_POINT ( 'NONE',  ( -3.636496289402156190, 16.53000000000001535, 11.19198476289190758 ) ) ;
#2106 = ORIENTED_EDGE ( 'NONE', *, *, #13611, .F. ) ;
#2107 = CARTESIAN_POINT ( 'NONE',  ( 11.76794919243112325, 70.43000000000000682, 1.441158131103945434E-15 ) ) ;
#2108 = CARTESIAN_POINT ( 'NONE',  ( -11.37499999999960743, -0.03437499999998146899, -4.711679271994912099 ) ) ;
#2109 = DIRECTION ( 'NONE',  ( 1.000000000000000000, 0.000000000000000000, 0.000000000000000000 ) ) ;
#2110 = CARTESIAN_POINT ( 'NONE',  ( -4.171729424061787483, -1.669999999999997931, -12.83926296998457417 ) ) ;
#2111 = CARTESIAN_POINT ( 'NONE',  ( -0.4699532509952931147, 43.19689778629660282, -13.49182028397187949 ) ) ;
#2112 = CARTESIAN_POINT ( 'NONE',  ( 3.456996083615943238, 76.05570077164072984, -13.05020998474081395 ) ) ;
#2113 = EDGE_CURVE ( 'NONE', #4811, #9433, #3784, .T. ) ;
#2114 = CARTESIAN_POINT ( 'NONE',  ( 13.16986379959834075, -81.16874999999980389, 13.16986379960055231 ) ) ;
#2115 = CARTESIAN_POINT ( 'NONE',  ( 3.099211176354089492, 65.79143792051837636, 13.13944202385564353 ) ) ;
#2116 = CARTESIAN_POINT ( 'NONE',  ( -10.92172942406178926, 79.63000000000000966, -7.935100905948389460 ) ) ;
#2117 = AXIS2_PLACEMENT_3D ( 'NONE', #6969, #60, #5464 ) ;
#2118 = CARTESIAN_POINT ( 'NONE',  ( -3.636496289402155746, 51.53000000000000114, 11.19198476289190936 ) ) ;
#2119 = CARTESIAN_POINT ( 'NONE',  ( -13.46443399275077368, 58.96388886014217690, 0.9794471126550197138 ) ) ;
#2120 = CARTESIAN_POINT ( 'NONE',  ( 12.97091200036834913, 45.29613835854244286, 3.742550467659857549 ) ) ;
#2121 = DIRECTION ( 'NONE',  ( -0.5000000000000005551, 0.000000000000000000, 0.8660254037844382635 ) ) ;
#2122 = DIRECTION ( 'NONE',  ( 0.000000000000000000, -1.000000000000000000, 0.000000000000000000 ) ) ;
#2123 = CARTESIAN_POINT ( 'NONE',  ( 13.49064639646111630, 30.44728826658618459, -0.5025169752740217266 ) ) ;
#2124 = CARTESIAN_POINT ( 'NONE',  ( -11.06336247766528480, 56.22163178693907071, 7.736410992500679207 ) ) ;
#2125 = DIRECTION ( 'NONE',  ( 0.000000000000000000, 0.000000000000000000, 1.000000000000000000 ) ) ;
#2126 = CARTESIAN_POINT ( 'NONE',  ( 8.065371710061997490, 63.87419627703715008, -10.82612419346579102 ) ) ;
#2127 = DIRECTION ( 'NONE',  ( 0.000000000000000000, 1.000000000000000000, 0.000000000000000000 ) ) ;
#2128 = CARTESIAN_POINT ( 'NONE',  ( 8.413557601958773446, 39.85841225840349011, -10.55875124266192522 ) ) ;
#2129 = ORIENTED_EDGE ( 'NONE', *, *, #8131, .F. ) ;
#2130 = CARTESIAN_POINT ( 'NONE',  ( -8.150177880934091235, 61.48915199108306240, -10.78270659849790647 ) ) ;
#2131 = VECTOR ( 'NONE', #10887, 1000.000000000000000 ) ;
#2132 = EDGE_LOOP ( 'NONE', ( #10988, #8282 ) ) ;
#2133 = ORIENTED_EDGE ( 'NONE', *, *, #9524, .F. ) ;
#2134 = CARTESIAN_POINT ( 'NONE',  ( -10.92172942406178926, 34.62999999999999545, -7.935100905948389460 ) ) ;
#2135 = CARTESIAN_POINT ( 'NONE',  ( -18.62500000000000000, -8.324999999999979750, -1.562973063126292555E-12 ) ) ;
#2136 = CARTESIAN_POINT ( 'NONE',  ( 12.61240584875263160, 48.25424400694961236, 4.854618120513341850 ) ) ;
#2137 =( BOUNDED_SURFACE ( )  B_SPLINE_SURFACE ( 1, 2, ( 
 ( #13118, #6161, #2143, #11537, #16916, #12944, #11626, #6326, #4908, #15661, #3569, #13033, #11713, #17089, #3662, #5986, #5090, #1181, #5176, #3749, #4007, #14854, #8179, #10567, #17434, #10482, #15842, #2398, #8093, #10820, #17264, #7833, #9251, #16014, #14772, #16098, #15928, #12138, #5430, #13372, #16182, #13292, #17178, #4094, #2748, #9509, #1343, #3920, #5347, #3837, #2662, #6592, #27, #14512, #1007, #6507, #13206, #14604, #6417, #2484, #7918, #11802, #11972, #17353, #13457, #11889, #6759, #5265, #10651, #9163, #1092, #9337, #14687, #2574, #8006, #9423, #1262, #6673, #12056, #10734, #8269, #211, #16636, #8535, #5879, #384, #11174, #11258, #10909, #6849, #9861, #1522, #8356, #13630, #4454, #5704, #4541, #3108, #15034, #3198, #1784, #1612, #16548, #14948, #7029, #11086, #5616, #9947, #10998, #15209, #12407, #13542, #5789, #12497, #6939, #3015, #7195, #15295, #16278, #7112, #12582, #16366, #13884, #470, #2838, #16459, #12318, #4184, #4274, #1432, #12227, #295, #119, #9683, #5525, #4361, #9771, #9596, #2926, #15116, #13714, #8445, #13799, #1698, #15704, #13972, #11344, #10604, #7787, #12665, #11842, #7282, #17217, #15970, #554, #3610, #1867, #17042, #3701, #1948, #957, #8704, #6279, #5128, #17303, #14064, #7694, #10519, #7373, #11923, #7869, #8618, #5964, #17128, #10034, #3289, #16720, #15882, #12751, #4627, #13072, #15382, #10348, #639, #6369, #11666, #4947, #15794, #9022, #14378, #2267, #11752, #5037, #1045, #2355, #10436, #9116, #14466, #13159, #6456, #3789, #9202, #14553, #2437, #13245, #1133, #6544, #2527, #6894, #4226, #7956, #14641, #13327, #5477, #16318, #1218, #9373, #6629, #2611, #12009, #9638, #6802, #17390, #1387, #16054, #2793, #16227, #14808, #8224, #5306, #2702, #13667, #1563, #10687, #3961, #14724, #8042, #5386, #13409, #8132, #4137, #13496, #12358, #1299, #10858, #6713, #12091, #12180, #9460, #3872, #13584, #14899, #72, #9549, #17474, #1478, #10771, #16135, #12267, #252, #4046, #11040, #14988, #165, #5569, #10952, #2880, #8312, #6983, #5657, #9288, #11389, #8398, #4404, #9724, #15160, #2969, #16761, #1819, #13752, #13925, #11126, #15336, #11297, #9902, #8660, #15069, #15249, #8748, #14106, #1651, #7067, #12449, #334, #423, #5743, #3147, #16675, #8573, #16500, #5917, #4668, #6095, #9814, #9989, #15426, #13838, #6006, #1907, #3059, #7235, #8487, #7152, #12536, #14016, #1990, #12621, #7324, #5830, #16411, #4493, #509, #4314, #11213, #4581, #16587, #12708, #596, #10075, #3334, #7416, #12798, #724, #6388, #16888, #7540, #3628, #16783, #15530, #12470, #3169, #7086, #4515, #8681, #7171, #5939, #13858, #11234, #4690, #4776, #1761, #12641, #10095, #12559, #16871, #12817, #3441 ),
 ( #15271, #444, #530, #5855, #11318, #10179, #357, #3263, #9837, #5763, #7257, #1843, #13773, #6028, #7350, #16698, #14040, #16611, #4603, #11146, #8594, #1927, #1672, #13946, #16522, #8770, #9923, #4429, #15445, #14125, #15183, #3084, #8509, #15357, #2011, #10009, #12729, #616, #11411, #3354, #7437, #704, #6114, #11495, #3522, #7789, #9118, #2269, #1046, #7521, #958, #1134, #6545, #16957, #4860, #10263, #15614, #10350, #8937, #11753, #14467, #17129, #14296, #15795, #14554, #8856, #2182, #2356, #13246, #6280, #15883, #11844, #7610, #5039, #12986, #869, #11668, #6457, #11924, #17219, #5129, #17043, #14209, #10520, #9203, #2095, #12902, #2438, #15705, #9024, #17305, #6895, #10773, #9289, #6631, #5658, #2794, #7958, #12268, #2529, #166, #3874, #13328, #16137, #14642, #12093, #16228, #14725, #13497, #3963, #1300, #5570, #12359, #9375, #2703, #10953, #2613, #6984, #2881, #1219, #12011, #12181, #5307, #16056, #17391, #16319, #8043, #10689, #8133, #13410, #5388, #4048, #6715, #9639, #14809, #4227, #17475, #1388, #6803, #10859, #253, #9550, #14989, #14900, #8225, #13585, #1479, #8313, #13668, #1564, #4315, #16676, #1652, #3239, #13839, #5918, #15250, #1820, #12451, #2970, #3148, #12800, #16502, #12622, #13753, #9903, #336, #7236, #11391, #510, #9725, #15071, #8400, #4670, #5745, #11298, #11128, #7068, #16588, #3061, #4406, #1909, #684, #6097, #8488, #15338, #9816, #15162, #1739, #6008, #8750, #7153, #12538, #425, #13926, #12710, #14018, #5831, #10076, #3336, #4582, #14108, #11214, #4494, #1992, #16413, #7418, #16763, #9991, #8662, #8574, #597, #7326, #15427, #16853, #771, #4755, #10161, #15510, #12883, #3422, #8837, #11477, #14195, #2077, #7502, #9396, #5324, #10794, #11123, #16498, #6345, #9617, #1454, #8468, #9530, #16479, #8378, #14968, #12159, #141, #6872, #5547, #16570, #7132, #5811, #315, #9792, #11194, #10838, #6781, #15139, #12247, #1542, #10931, #3037, #5637, #4476, #12519, #9706, #14873, #16298, #16204, #403, #2859, #1364, #231, #4115, #12339, #11019, #16390, #9882, #50, #1632, #2768, #12429, #15231, #3128, #13477, #6160, #2059, #11454, #14171, #8640, #7394, #7214, #8724, #16915, #4907, #12774, #15660, #2142, #13991, #491, #4820, #7567, #5897, #11277, #4561, #10136, #828, #9967, #1888, #3218, #7302, #5985, #6239, #16828, #11367, #3400, #10053, #10221, #15574, #662, #15403, #11712, #17263, #1261, #4995, #9073, #1006, #3748, #14511, #5175, #12317, #15033, #13713, #9770, #3014, #8444, #1697, #383, #12496, #5788, #4006, #14771, #8092, #13456, #5878, #8703, #3197, #13883, #7281, #3378, #11173, #4626, #15468, #4540, #15208, #10033, #7372, #7194, #11257, #638, #12664, #553, #5963 ) ),
 .UNSPECIFIED., .F., .F., .T. ) 
 B_SPLINE_SURFACE_WITH_KNOTS ( ( 2, 2 ),
 ( 3, 2, 2, 2, 2, 2, 2, 2, 2, 2, 2, 2, 2, 2, 2, 2, 2, 2, 2, 2, 2, 2, 2, 2, 2, 2, 2, 2, 2, 2, 2, 2, 2, 2, 2, 2, 2, 2, 2, 2, 2, 2, 2, 2, 2, 2, 2, 2, 2, 2, 2, 2, 2, 2, 2, 2, 2, 2, 2, 2, 2, 2, 2, 2, 2, 2, 2, 2, 2, 2, 2, 2, 2, 2, 2, 2, 2, 2, 2, 2, 2, 2, 2, 2, 2, 2, 2, 2, 2, 2, 2, 2, 2, 2, 2, 2, 2, 2, 2, 2, 2, 2, 2, 2, 2, 2, 2, 2, 2, 2, 2, 2, 2, 2, 2, 2, 2, 2, 2, 2, 2, 2, 2, 2, 2, 2, 2, 2, 2, 2, 2, 2, 2, 2, 2, 2, 2, 2, 2, 2, 2, 2, 2, 2, 2, 2, 2, 2, 2, 2, 2, 2, 2, 2, 2, 2, 2, 2, 2, 2, 2, 2, 2, 2, 2, 2, 2, 2, 2, 2, 2, 2, 2, 2, 2, 2, 2, 2, 3 ),
 ( 0.000000000000000000, 1.000000000000000000 ),
 ( 0.000000000000000000, 0.005555555555555555768, 0.01111111111111111154, 0.01666666666666666644, 0.02222222222222222307, 0.02777777777777777624, 0.03333333333333333287, 0.03888888888888888951, 0.04444444444444444614, 0.05000000000000000278, 0.05555555555555555247, 0.06111111111111110911, 0.06666666666666666574, 0.07222222222222221544, 0.07777777777777777901, 0.08333333333333332871, 0.08888888888888889228, 0.09444444444444444198, 0.1000000000000000056, 0.1055555555555555552, 0.1111111111111111049, 0.1166666666666666685, 0.1222222222222222182, 0.1277777777777777679, 0.1333333333333333315, 0.1388888888888888951, 0.1444444444444444309, 0.1499999999999999944, 0.1555555555555555580, 0.1611111111111111216, 0.1666666666666666574, 0.1722222222222222210, 0.1777777777777777846, 0.1833333333333333204, 0.1888888888888888840, 0.1944444444444444475, 0.2000000000000000111, 0.2055555555555555469, 0.2111111111111111105, 0.2166666666666666741, 0.2222222222222222099, 0.2277777777777777735, 0.2333333333333333370, 0.2388888888888889006, 0.2444444444444444364, 0.2500000000000000000, 0.2555555555555555358, 0.2611111111111111271, 0.2666666666666666630, 0.2722222222222221988, 0.2777777777777777901, 0.2833333333333333259, 0.2888888888888888618, 0.2944444444444444531, 0.2999999999999999889, 0.3055555555555555802, 0.3111111111111111160, 0.3166666666666666519, 0.3222222222222222432, 0.3277777777777777790, 0.3333333333333333148, 0.3388888888888889062, 0.3444444444444444420, 0.3499999999999999778, 0.3555555555555555691, 0.3611111111111111049, 0.3666666666666666408, 0.3722222222222222321, 0.3777777777777777679, 0.3833333333333333592, 0.3888888888888888951, 0.3944444444444444309, 0.4000000000000000222, 0.4055555555555555580, 0.4111111111111110938, 0.4166666666666666852, 0.4222222222222222210, 0.4277777777777777568, 0.4333333333333333481, 0.4388888888888888840, 0.4444444444444444198, 0.4500000000000000111, 0.4555555555555555469, 0.4611111111111111382, 0.4666666666666666741, 0.4722222222222222099, 0.4777777777777778012, 0.4833333333333333370, 0.4888888888888888729, 0.4944444444444444642, 0.5000000000000000000, 0.5055555555555555358, 0.5111111111111110716, 0.5166666666666667185, 0.5222222222222222543, 0.5277777777777777901, 0.5333333333333333259, 0.5388888888888888618, 0.5444444444444443976, 0.5500000000000000444, 0.5555555555555555802, 0.5611111111111111160, 0.5666666666666666519, 0.5722222222222221877, 0.5777777777777777235, 0.5833333333333333703, 0.5888888888888889062, 0.5944444444444444420, 0.5999999999999999778, 0.6055555555555555136, 0.6111111111111111605, 0.6166666666666666963, 0.6222222222222222321, 0.6277777777777777679, 0.6333333333333333037, 0.6388888888888888395, 0.6444444444444444864, 0.6500000000000000222, 0.6555555555555555580, 0.6611111111111110938, 0.6666666666666666297, 0.6722222222222222765, 0.6777777777777778123, 0.6833333333333333481, 0.6888888888888888840, 0.6944444444444444198, 0.6999999999999999556, 0.7055555555555556024, 0.7111111111111111382, 0.7166666666666666741, 0.7222222222222222099, 0.7277777777777777457, 0.7333333333333332815, 0.7388888888888889284, 0.7444444444444444642, 0.7500000000000000000, 0.7555555555555555358, 0.7611111111111110716, 0.7666666666666667185, 0.7722222222222222543, 0.7777777777777777901, 0.7833333333333333259, 0.7888888888888888618, 0.7944444444444443976, 0.8000000000000000444, 0.8055555555555555802, 0.8111111111111111160, 0.8166666666666666519, 0.8222222222222221877, 0.8277777777777777235, 0.8333333333333333703, 0.8388888888888889062, 0.8444444444444444420, 0.8499999999999999778, 0.8555555555555555136, 0.8611111111111111605, 0.8666666666666666963, 0.8722222222222222321, 0.8777777777777777679, 0.8833333333333333037, 0.8888888888888888395, 0.8944444444444444864, 0.9000000000000000222, 0.9055555555555555580, 0.9111111111111110938, 0.9166666666666666297, 0.9222222222222222765, 0.9277777777777778123, 0.9333333333333333481, 0.9388888888888888840, 0.9444444444444444198, 0.9499999999999999556, 0.9555555555555556024, 0.9611111111111111382, 0.9666666666666666741, 0.9722222222222222099, 0.9777777777777777457, 0.9814746766279994761, 0.9912894233942795008 ),
 .UNSPECIFIED. ) 
 GEOMETRIC_REPRESENTATION_ITEM ( )  RATIONAL_B_SPLINE_SURFACE ( (
 ( 1.000000000000000000, 0.9510565162951535312, 1.000000000000000000, 0.9510565162951535312, 1.000000000000000000, 0.9510565162951535312, 1.000000000000000000, 0.9510565162951535312, 1.000000000000000000, 0.9510565162951535312, 1.000000000000000000, 0.9510565162951535312, 1.000000000000000000, 0.9510565162951535312, 1.000000000000000000, 0.9510565162951535312, 1.000000000000000000, 0.9510565162951535312, 1.000000000000000000, 0.9510565162951535312, 1.000000000000000000, 0.9510565162951535312, 1.000000000000000000, 0.9510565162951535312, 1.000000000000000000, 0.9510565162951535312, 1.000000000000000000, 0.9510565162951535312, 1.000000000000000000, 0.9510565162951535312, 1.000000000000000000, 0.9510565162951535312, 1.000000000000000000, 0.9510565162951535312, 1.000000000000000000, 0.9510565162951535312, 1.000000000000000000, 0.9510565162951535312, 1.000000000000000000, 0.9510565162951535312, 1.000000000000000000, 0.9510565162951535312, 1.000000000000000000, 0.9510565162951535312, 1.000000000000000000, 0.9510565162951535312, 1.000000000000000000, 0.9510565162951535312, 1.000000000000000000, 0.9510565162951535312, 1.000000000000000000, 0.9510565162951535312, 1.000000000000000000, 0.9510565162951535312, 1.000000000000000000, 0.9510565162951535312, 1.000000000000000000, 0.9510565162951535312, 1.000000000000000000, 0.9510565162951535312, 1.000000000000000000, 0.9510565162951535312, 1.000000000000000000, 0.9510565162951535312, 1.000000000000000000, 0.9510565162951535312, 1.000000000000000000, 0.9510565162951535312, 1.000000000000000000, 0.9510565162951535312, 1.000000000000000000, 0.9510565162951535312, 1.000000000000000000, 0.9510565162951535312, 1.000000000000000000, 0.9510565162951535312, 1.000000000000000000, 0.9510565162951535312, 1.000000000000000000, 0.9510565162951535312, 1.000000000000000000, 0.9510565162951535312, 1.000000000000000000, 0.9510565162951535312, 1.000000000000000000, 0.9510565162951535312, 1.000000000000000000, 0.9510565162951535312, 1.000000000000000000, 0.9510565162951535312, 1.000000000000000000, 0.9510565162951535312, 1.000000000000000000, 0.9510565162951535312, 1.000000000000000000, 0.9510565162951535312, 1.000000000000000000, 0.9510565162951535312, 1.000000000000000000, 0.9510565162951535312, 1.000000000000000000, 0.9510565162951535312, 1.000000000000000000, 0.9510565162951535312, 1.000000000000000000, 0.9510565162951535312, 1.000000000000000000, 0.9510565162951535312, 1.000000000000000000, 0.9510565162951535312, 1.000000000000000000, 0.9510565162951535312, 1.000000000000000000, 0.9510565162951535312, 1.000000000000000000, 0.9510565162951535312, 1.000000000000000000, 0.9510565162951535312, 1.000000000000000000, 0.9510565162951535312, 1.000000000000000000, 0.9510565162951535312, 1.000000000000000000, 0.9510565162951535312, 1.000000000000000000, 0.9510565162951535312, 1.000000000000000000, 0.9510565162951535312, 1.000000000000000000, 0.9510565162951535312, 1.000000000000000000, 0.9510565162951535312, 1.000000000000000000, 0.9510565162951535312, 1.000000000000000000, 0.9510565162951535312, 1.000000000000000000, 0.9510565162951535312, 1.000000000000000000, 0.9510565162951535312, 1.000000000000000000, 0.9510565162951535312, 1.000000000000000000, 0.9510565162951535312, 1.000000000000000000, 0.9510565162951535312, 1.000000000000000000, 0.9510565162951535312, 1.000000000000000000, 0.9510565162951535312, 1.000000000000000000, 0.9510565162951535312, 1.000000000000000000, 0.9510565162951535312, 1.000000000000000000, 0.9510565162951535312, 1.000000000000000000, 0.9510565162951535312, 1.000000000000000000, 0.9510565162951535312, 1.000000000000000000, 0.9510565162951535312, 1.000000000000000000, 0.9510565162951535312, 1.000000000000000000, 0.9510565162951535312, 1.000000000000000000, 0.9510565162951535312, 1.000000000000000000, 0.9510565162951535312, 1.000000000000000000, 0.9510565162951535312, 1.000000000000000000, 0.9510565162951535312, 1.000000000000000000, 0.9510565162951535312, 1.000000000000000000, 0.9510565162951535312, 1.000000000000000000, 0.9510565162951535312, 1.000000000000000000, 0.9510565162951535312, 1.000000000000000000, 0.9510565162951535312, 1.000000000000000000, 0.9510565162951535312, 1.000000000000000000, 0.9510565162951535312, 1.000000000000000000, 0.9510565162951535312, 1.000000000000000000, 0.9510565162951535312, 1.000000000000000000, 0.9510565162951535312, 1.000000000000000000, 0.9510565162951535312, 1.000000000000000000, 0.9510565162951535312, 1.000000000000000000, 0.9510565162951535312, 1.000000000000000000, 0.9510565162951535312, 1.000000000000000000, 0.9510565162951535312, 1.000000000000000000, 0.9510565162951535312, 1.000000000000000000, 0.9510565162951535312, 1.000000000000000000, 0.9510565162951535312, 1.000000000000000000, 0.9510565162951535312, 1.000000000000000000, 0.9510565162951535312, 1.000000000000000000, 0.9510565162951535312, 1.000000000000000000, 0.9510565162951535312, 1.000000000000000000, 0.9510565162951535312, 1.000000000000000000, 0.9510565162951535312, 1.000000000000000000, 0.9510565162951535312, 1.000000000000000000, 0.9510565162951535312, 1.000000000000000000, 0.9510565162951535312, 1.000000000000000000, 0.9510565162951535312, 1.000000000000000000, 0.9510565162951535312, 1.000000000000000000, 0.9510565162951535312, 1.000000000000000000, 0.9510565162951535312, 1.000000000000000000, 0.9510565162951535312, 1.000000000000000000, 0.9510565162951535312, 1.000000000000000000, 0.9510565162951535312, 1.000000000000000000, 0.9510565162951535312, 1.000000000000000000, 0.9510565162951535312, 1.000000000000000000, 0.9510565162951535312, 1.000000000000000000, 0.9510565162951535312, 1.000000000000000000, 0.9510565162951535312, 1.000000000000000000, 0.9510565162951535312, 1.000000000000000000, 0.9510565162951535312, 1.000000000000000000, 0.9510565162951535312, 1.000000000000000000, 0.9510565162951535312, 1.000000000000000000, 0.9510565162951535312, 1.000000000000000000, 0.9510565162951535312, 1.000000000000000000, 0.9510565162951535312, 1.000000000000000000, 0.9510565162951535312, 1.000000000000000000, 0.9510565162951535312, 1.000000000000000000, 0.9510565162951535312, 1.000000000000000000, 0.9510565162951535312, 1.000000000000000000, 0.9510565162951535312, 1.000000000000000000, 0.9510565162951535312, 1.000000000000000000, 0.9510565162951535312, 1.000000000000000000, 0.9510565162951535312, 1.000000000000000000, 0.9510565162951535312, 1.000000000000000000, 0.9510565162951535312, 1.000000000000000000, 0.9510565162951535312, 1.000000000000000000, 0.9510565162951535312, 1.000000000000000000, 0.9510565162951535312, 1.000000000000000000, 0.9510565162951535312, 1.000000000000000000, 0.9510565162951535312, 1.000000000000000000, 0.9510565162951535312, 1.000000000000000000, 0.9510565162951535312, 1.000000000000000000, 0.9510565162951535312, 1.000000000000000000, 0.9510565162951535312, 1.000000000000000000, 0.9510565162951535312, 1.000000000000000000, 0.9510565162951535312, 1.000000000000000000, 0.9510565162951535312, 1.000000000000000000, 0.9510565162951535312, 1.000000000000000000, 0.9510565162951535312, 1.000000000000000000, 0.9510565162951535312, 1.000000000000000000, 0.9510565162951535312, 1.000000000000000000, 0.9510565162951535312, 1.000000000000000000, 0.9510565162951535312, 1.000000000000000000, 0.9510565162951535312, 1.000000000000000000, 0.9510565162951535312, 1.000000000000000000, 0.9510565162951535312, 1.000000000000000000, 0.9510565162951535312, 1.000000000000000000, 0.9510565162951535312, 1.000000000000000000, 0.9510565162951535312, 1.000000000000000000, 0.9510565162951535312, 1.000000000000000000, 0.9510565162951535312, 1.000000000000000000, 0.9510565162951535312, 1.000000000000000000, 0.9510565162951535312, 1.000000000000000000, 0.9510565162951535312, 1.000000000000000000, 0.9510565162951535312, 1.000000000000000000, 0.9510565162951535312, 1.000000000000000000, 0.9510565162951535312, 1.000000000000000000, 0.9510565162951535312, 1.000000000000000000, 0.9674309604458272149, 0.9782075210486875783, 0.9782075210486875783, 0.9782075210486875783),
 ( 1.000000000000000000, 0.9510565162951535312, 1.000000000000000000, 0.9510565162951535312, 1.000000000000000000, 0.9510565162951535312, 1.000000000000000000, 0.9510565162951535312, 1.000000000000000000, 0.9510565162951535312, 1.000000000000000000, 0.9510565162951535312, 1.000000000000000000, 0.9510565162951535312, 1.000000000000000000, 0.9510565162951535312, 1.000000000000000000, 0.9510565162951535312, 1.000000000000000000, 0.9510565162951535312, 1.000000000000000000, 0.9510565162951535312, 1.000000000000000000, 0.9510565162951535312, 1.000000000000000000, 0.9510565162951535312, 1.000000000000000000, 0.9510565162951535312, 1.000000000000000000, 0.9510565162951535312, 1.000000000000000000, 0.9510565162951535312, 1.000000000000000000, 0.9510565162951535312, 1.000000000000000000, 0.9510565162951535312, 1.000000000000000000, 0.9510565162951535312, 1.000000000000000000, 0.9510565162951535312, 1.000000000000000000, 0.9510565162951535312, 1.000000000000000000, 0.9510565162951535312, 1.000000000000000000, 0.9510565162951535312, 1.000000000000000000, 0.9510565162951535312, 1.000000000000000000, 0.9510565162951535312, 1.000000000000000000, 0.9510565162951535312, 1.000000000000000000, 0.9510565162951535312, 1.000000000000000000, 0.9510565162951535312, 1.000000000000000000, 0.9510565162951535312, 1.000000000000000000, 0.9510565162951535312, 1.000000000000000000, 0.9510565162951535312, 1.000000000000000000, 0.9510565162951535312, 1.000000000000000000, 0.9510565162951535312, 1.000000000000000000, 0.9510565162951535312, 1.000000000000000000, 0.9510565162951535312, 1.000000000000000000, 0.9510565162951535312, 1.000000000000000000, 0.9510565162951535312, 1.000000000000000000, 0.9510565162951535312, 1.000000000000000000, 0.9510565162951535312, 1.000000000000000000, 0.9510565162951535312, 1.000000000000000000, 0.9510565162951535312, 1.000000000000000000, 0.9510565162951535312, 1.000000000000000000, 0.9510565162951535312, 1.000000000000000000, 0.9510565162951535312, 1.000000000000000000, 0.9510565162951535312, 1.000000000000000000, 0.9510565162951535312, 1.000000000000000000, 0.9510565162951535312, 1.000000000000000000, 0.9510565162951535312, 1.000000000000000000, 0.9510565162951535312, 1.000000000000000000, 0.9510565162951535312, 1.000000000000000000, 0.9510565162951535312, 1.000000000000000000, 0.9510565162951535312, 1.000000000000000000, 0.9510565162951535312, 1.000000000000000000, 0.9510565162951535312, 1.000000000000000000, 0.9510565162951535312, 1.000000000000000000, 0.9510565162951535312, 1.000000000000000000, 0.9510565162951535312, 1.000000000000000000, 0.9510565162951535312, 1.000000000000000000, 0.9510565162951535312, 1.000000000000000000, 0.9510565162951535312, 1.000000000000000000, 0.9510565162951535312, 1.000000000000000000, 0.9510565162951535312, 1.000000000000000000, 0.9510565162951535312, 1.000000000000000000, 0.9510565162951535312, 1.000000000000000000, 0.9510565162951535312, 1.000000000000000000, 0.9510565162951535312, 1.000000000000000000, 0.9510565162951535312, 1.000000000000000000, 0.9510565162951535312, 1.000000000000000000, 0.9510565162951535312, 1.000000000000000000, 0.9510565162951535312, 1.000000000000000000, 0.9510565162951535312, 1.000000000000000000, 0.9510565162951535312, 1.000000000000000000, 0.9510565162951535312, 1.000000000000000000, 0.9510565162951535312, 1.000000000000000000, 0.9510565162951535312, 1.000000000000000000, 0.9510565162951535312, 1.000000000000000000, 0.9510565162951535312, 1.000000000000000000, 0.9510565162951535312, 1.000000000000000000, 0.9510565162951535312, 1.000000000000000000, 0.9510565162951535312, 1.000000000000000000, 0.9510565162951535312, 1.000000000000000000, 0.9510565162951535312, 1.000000000000000000, 0.9510565162951535312, 1.000000000000000000, 0.9510565162951535312, 1.000000000000000000, 0.9510565162951535312, 1.000000000000000000, 0.9510565162951535312, 1.000000000000000000, 0.9510565162951535312, 1.000000000000000000, 0.9510565162951535312, 1.000000000000000000, 0.9510565162951535312, 1.000000000000000000, 0.9510565162951535312, 1.000000000000000000, 0.9510565162951535312, 1.000000000000000000, 0.9510565162951535312, 1.000000000000000000, 0.9510565162951535312, 1.000000000000000000, 0.9510565162951535312, 1.000000000000000000, 0.9510565162951535312, 1.000000000000000000, 0.9510565162951535312, 1.000000000000000000, 0.9510565162951535312, 1.000000000000000000, 0.9510565162951535312, 1.000000000000000000, 0.9510565162951535312, 1.000000000000000000, 0.9510565162951535312, 1.000000000000000000, 0.9510565162951535312, 1.000000000000000000, 0.9510565162951535312, 1.000000000000000000, 0.9510565162951535312, 1.000000000000000000, 0.9510565162951535312, 1.000000000000000000, 0.9510565162951535312, 1.000000000000000000, 0.9510565162951535312, 1.000000000000000000, 0.9510565162951535312, 1.000000000000000000, 0.9510565162951535312, 1.000000000000000000, 0.9510565162951535312, 1.000000000000000000, 0.9510565162951535312, 1.000000000000000000, 0.9510565162951535312, 1.000000000000000000, 0.9510565162951535312, 1.000000000000000000, 0.9510565162951535312, 1.000000000000000000, 0.9510565162951535312, 1.000000000000000000, 0.9510565162951535312, 1.000000000000000000, 0.9510565162951535312, 1.000000000000000000, 0.9510565162951535312, 1.000000000000000000, 0.9510565162951535312, 1.000000000000000000, 0.9510565162951535312, 1.000000000000000000, 0.9510565162951535312, 1.000000000000000000, 0.9510565162951535312, 1.000000000000000000, 0.9510565162951535312, 1.000000000000000000, 0.9510565162951535312, 1.000000000000000000, 0.9510565162951535312, 1.000000000000000000, 0.9510565162951535312, 1.000000000000000000, 0.9510565162951535312, 1.000000000000000000, 0.9510565162951535312, 1.000000000000000000, 0.9510565162951535312, 1.000000000000000000, 0.9510565162951535312, 1.000000000000000000, 0.9510565162951535312, 1.000000000000000000, 0.9510565162951535312, 1.000000000000000000, 0.9510565162951535312, 1.000000000000000000, 0.9510565162951535312, 1.000000000000000000, 0.9510565162951535312, 1.000000000000000000, 0.9510565162951535312, 1.000000000000000000, 0.9510565162951535312, 1.000000000000000000, 0.9510565162951535312, 1.000000000000000000, 0.9510565162951535312, 1.000000000000000000, 0.9510565162951535312, 1.000000000000000000, 0.9510565162951535312, 1.000000000000000000, 0.9510565162951535312, 1.000000000000000000, 0.9510565162951535312, 1.000000000000000000, 0.9510565162951535312, 1.000000000000000000, 0.9510565162951535312, 1.000000000000000000, 0.9510565162951535312, 1.000000000000000000, 0.9510565162951535312, 1.000000000000000000, 0.9510565162951535312, 1.000000000000000000, 0.9510565162951535312, 1.000000000000000000, 0.9510565162951535312, 1.000000000000000000, 0.9510565162951535312, 1.000000000000000000, 0.9510565162951535312, 1.000000000000000000, 0.9510565162951535312, 1.000000000000000000, 0.9510565162951535312, 1.000000000000000000, 0.9510565162951535312, 1.000000000000000000, 0.9510565162951535312, 1.000000000000000000, 0.9510565162951535312, 1.000000000000000000, 0.9510565162951535312, 1.000000000000000000, 0.9510565162951535312, 1.000000000000000000, 0.9510565162951535312, 1.000000000000000000, 0.9510565162951535312, 1.000000000000000000, 0.9510565162951535312, 1.000000000000000000, 0.9510565162951535312, 1.000000000000000000, 0.9510565162951535312, 1.000000000000000000, 0.9510565162951535312, 1.000000000000000000, 0.9510565162951535312, 1.000000000000000000, 0.9510565162951535312, 1.000000000000000000, 0.9510565162951535312, 1.000000000000000000, 0.9510565162951535312, 1.000000000000000000, 0.9510565162951535312, 1.000000000000000000, 0.9510565162951535312, 1.000000000000000000, 0.9510565162951535312, 1.000000000000000000, 0.9510565162951535312, 1.000000000000000000, 0.9510565162951535312, 1.000000000000000000, 0.9510565162951535312, 1.000000000000000000, 0.9510565162951535312, 1.000000000000000000, 0.9510565162951535312, 1.000000000000000000, 0.9674309604458272149, 0.9782075210486875783, 0.9782075210486875783, 0.9782075210486875783) ) ) 
 REPRESENTATION_ITEM ( '' )  SURFACE ( )  );
#2138 = ADVANCED_FACE ( 'NONE', ( #7657 ), #2137, .T. ) ;
#2139 = CARTESIAN_POINT ( 'NONE',  ( 2.279044047469930501, 58.09805576578575170, -13.30646307545504392 ) ) ;
#2140 = CARTESIAN_POINT ( 'NONE',  ( 10.96618175729265054, 78.72740224806844367, -7.873708902144001875 ) ) ;
#2141 = CARTESIAN_POINT ( 'NONE',  ( 9.520470885617717371, 76.73000000000000398, -6.917026985038131848 ) ) ;
#2142 = CARTESIAN_POINT ( 'NONE',  ( 13.49999999999999822, 41.28000000000000114, 4.386415899144237684 ) ) ;
#2143 = CARTESIAN_POINT ( 'NONE',  ( -9.520470885617715595, 83.62999999999999545, -6.917026985038136289 ) ) ;
#2144 = CARTESIAN_POINT ( 'NONE',  ( -0.3003120841998243029, 47.66920191232892279, 13.49667088445732688 ) ) ;
#2145 = CIRCLE ( 'NONE', #8670, 12.00000000000000178 ) ;
#2146 = CARTESIAN_POINT ( 'NONE',  ( 8.343458848123580296, 40.97999999999998977, 11.48378591275253768 ) ) ;
#2147 = CARTESIAN_POINT ( 'NONE',  ( -0.1072688110503501047, 67.18385698782702775, -13.49957998319009711 ) ) ;
#2148 = CARTESIAN_POINT ( 'NONE',  ( 8.043339635996302306, -23.96874999999992539, 8.043339635997654113 ) ) ;
#2149 = CARTESIAN_POINT ( 'NONE',  ( -13.50000000000000000, 78.93000000000000682, -3.306546357697853733E-15 ) ) ;
#2150 = CARTESIAN_POINT ( 'NONE',  ( 10.33907932670936169, 33.76270983375775359, -8.680815796010884711 ) ) ;
#2151 = ORIENTED_EDGE ( 'NONE', *, *, #3966, .F. ) ;
#2152 = DIRECTION ( 'NONE',  ( 0.000000000000000000, 0.000000000000000000, -1.000000000000000000 ) ) ;
#2153 = ORIENTED_EDGE ( 'NONE', *, *, #15578, .F. ) ;
#2154 = CARTESIAN_POINT ( 'NONE',  ( 5.313600336010172676, 66.98769782423862296, -12.41030752995400377 ) ) ;
#2155 = CARTESIAN_POINT ( 'NONE',  ( 11.37499999999999645, -40.54999999999992610, 9.531744055041752924E-13 ) ) ;
#2156 = CARTESIAN_POINT ( 'NONE',  ( 0.000000000000000000, 0.000000000000000000, 0.000000000000000000 ) ) ;
#2157 = CARTESIAN_POINT ( 'NONE',  ( -7.125339594746328942, 59.41507076714115243, 11.46659377414734493 ) ) ;
#2158 = DIRECTION ( 'NONE',  ( -1.000000000000000000, -0.000000000000000000, -0.000000000000000000 ) ) ;
#2159 = FACE_OUTER_BOUND ( 'NONE', #12436, .T. ) ;
#2160 = CARTESIAN_POINT ( 'NONE',  ( 7.441533999091377360, 71.95841347386840425, 11.26395245896506658 ) ) ;
#2161 = CARTESIAN_POINT ( 'NONE',  ( 2.607531440858944223E-15, 52.17999999999998550, -14.19474002721660355 ) ) ;
#2162 = CARTESIAN_POINT ( 'NONE',  ( 2.000520122481862502E-14, 73.67999999999999261, 13.50000000000000000 ) ) ;
#2163 = DIRECTION ( 'NONE',  ( -0.000000000000000000, 1.000000000000000000, -0.000000000000000000 ) ) ;
#2164 = CARTESIAN_POINT ( 'NONE',  ( -13.16986379960055231, -77.00624999999982379, 13.16986379959834252 ) ) ;
#2165 = CARTESIAN_POINT ( 'NONE',  ( -11.60114662261267071, 68.18707878082513218, 6.904087372892822039 ) ) ;
#2166 = CARTESIAN_POINT ( 'NONE',  ( 7.714727599197338748, -63.47812499999984226, 18.62500000000063949 ) ) ;
#2167 = CARTESIAN_POINT ( 'NONE',  ( 1.124411942366441597, 55.13962006267097848, -13.46143473974375304 ) ) ;
#2168 = CARTESIAN_POINT ( 'NONE',  ( -18.62500000000000000, -24.97499999999994102, -1.562973063126292555E-12 ) ) ;
#2169 = CARTESIAN_POINT ( 'NONE',  ( -2.487099657241000017, 65.59057316322061126, 13.26893666242352054 ) ) ;
#2170 = CARTESIAN_POINT ( 'NONE',  ( 12.00000000000000178, 8.296025403784431873, 1.734723475976807094E-15 ) ) ;
#2171 = CARTESIAN_POINT ( 'NONE',  ( 9.352804080103156892, 8.052183443614390868, -15.42355852573366448 ) ) ;
#2172 = CARTESIAN_POINT ( 'NONE',  ( 2.621994543952811015E-15, 26.18000000000001037, -14.19474002721660355 ) ) ;
#2173 = ORIENTED_EDGE ( 'NONE', *, *, #16812, .T. ) ;
#2174 = CARTESIAN_POINT ( 'NONE',  ( -2.138190073780635636, 9.603118573027019877, 13.49999995795558760 ) ) ;
#2175 = CARTESIAN_POINT ( 'NONE',  ( 13.50000000000000000, 80.43000000000000682, 1.653273178848926867E-15 ) ) ;
#2176 = CARTESIAN_POINT ( 'NONE',  ( -12.54118595349893361, 32.11158997754159827, 4.998678152965537969 ) ) ;
#2177 = CARTESIAN_POINT ( 'NONE',  ( 3.692898783743682856, 74.81278297373158637, 12.98509198411088228 ) ) ;
#2178 = CARTESIAN_POINT ( 'NONE',  ( 11.65057582055373864, 60.17622677577021761, 6.820123597281462224 ) ) ;
#2179 = CARTESIAN_POINT ( 'NONE',  ( 10.92172942406178926, -1.869999999999996554, 7.935100905948385908 ) ) ;
#2180 = CARTESIAN_POINT ( 'NONE',  ( 13.50000000000000355, 62.57999999999999829, -4.386415899144233244 ) ) ;
#2181 = CARTESIAN_POINT ( 'NONE',  ( 690.7486963872877368, 879.4553902717701703, 1297.674793841596738 ) ) ;
#2182 = CARTESIAN_POINT ( 'NONE',  ( 4.171729424061791924, 75.03000000000000114, -12.83926296998457239 ) ) ;
#2183 = CARTESIAN_POINT ( 'NONE',  ( 12.63195413649815535, 51.60251507868900944, -4.762774090562415630 ) ) ;
#2184 = CARTESIAN_POINT ( 'NONE',  ( -13.47802306467995059, 37.90338780716024303, -0.7702094408733768383 ) ) ;
#2185 = CARTESIAN_POINT ( 'NONE',  ( 13.03650423020505400, 36.55508012865420397, -3.507091010788072616 ) ) ;
#2186 = CARTESIAN_POINT ( 'NONE',  ( -11.37499999999960210, -31.18437499999994245, -4.711679271994911211 ) ) ;
#2187 = EDGE_CURVE ( 'NONE', #13170, #1168, #11343, .T. ) ;
#2188 = CARTESIAN_POINT ( 'NONE',  ( -3.365647742148276667, 74.55898446082595399, 13.07385443055280660 ) ) ;
#2189 = CARTESIAN_POINT ( 'NONE',  ( -10.65461094870909164, 77.24527756324417282, 8.290314445817193345 ) ) ;
#2190 = CARTESIAN_POINT ( 'NONE',  ( -10.92172942406179104, 61.22999999999999687, 7.935100905948387684 ) ) ;
#2191 = CARTESIAN_POINT ( 'NONE',  ( 8.190734026114112609, 41.99145286735084426, 10.73174394289365985 ) ) ;
#2192 = ORIENTED_EDGE ( 'NONE', *, *, #2367, .T. ) ;
#2193 = CARTESIAN_POINT ( 'NONE',  ( -11.76794919243112325, 12.78000000000000824, -3.823638476888998827 ) ) ;
#2194 = EDGE_LOOP ( 'NONE', ( #4958, #7926, #1806, #8990 ) ) ;
#2195 = CARTESIAN_POINT ( 'NONE',  ( -9.520470885617715595, 59.63000000000000256, -6.917026985038136289 ) ) ;
#2196 = CARTESIAN_POINT ( 'NONE',  ( 11.37499999999960565, -74.95937499999980957, 4.711679271994918317 ) ) ;
#2197 = DIRECTION ( 'NONE',  ( -0.000000000000000000, -1.000000000000000000, -0.000000000000000000 ) ) ;
#2198 = CARTESIAN_POINT ( 'NONE',  ( 4.171729424061789260, -0.1700000000000034817, 12.83926296998457239 ) ) ;
#2199 = CARTESIAN_POINT ( 'NONE',  ( 3.635492542842543084, 76.04928109828082938, -13.00127780319107806 ) ) ;
#2200 = AXIS2_PLACEMENT_3D ( 'NONE', #10850, #17382, #2518 ) ;
#2201 = CARTESIAN_POINT ( 'NONE',  ( -1.564113515457998572E-12, -62.43749999999985079, 18.62500000000000000 ) ) ;
#2202 = CARTESIAN_POINT ( 'NONE',  ( 3.145715289543748128, 65.79306979106382869, 13.12842161919002670 ) ) ;
#2203 = CARTESIAN_POINT ( 'NONE',  ( 13.50000000000000355, 78.57999999999999829, -4.386415899144233244 ) ) ;
#2204 = CARTESIAN_POINT ( 'NONE',  ( -7.272992578804307939, 53.47999999999998977, -10.01041549318726886 ) ) ;
#2205 = DIRECTION ( 'NONE',  ( 1.000000000000000000, 0.000000000000000000, 0.000000000000000000 ) ) ;
#2206 = CARTESIAN_POINT ( 'NONE',  ( -11.02082988299614286, 59.22417995457187345, 7.797019995292360228 ) ) ;
#2207 = CARTESIAN_POINT ( 'NONE',  ( 11.48013075663052085, 45.16464998993217250, 7.103285909153894906 ) ) ;
#2208 = CARTESIAN_POINT ( 'NONE',  ( 13.49953346300133106, 69.46047903813546043, -0.8869165812264260262 ) ) ;
#2209 = CARTESIAN_POINT ( 'NONE',  ( 0.000000000000000000, 9.000000000000000000, 0.000000000000000000 ) ) ;
#2210 = CARTESIAN_POINT ( 'NONE',  ( 13.48560614430077997, 30.45153926847759962, -0.6251654576716944023 ) ) ;
#2211 = CARTESIAN_POINT ( 'NONE',  ( -13.47260917658593193, 55.90032134080831838, -0.8602528088475849266 ) ) ;
#2212 = EDGE_CURVE ( 'NONE', #6426, #3760, #8836, .T. ) ;
#2213 = CARTESIAN_POINT ( 'NONE',  ( -9.432887964969109973, 50.30984541438331092, 9.660289610433199670 ) ) ;
#2214 = CARTESIAN_POINT ( 'NONE',  ( -8.697098998243532012E-15, 64.18000000000002103, -13.50000000000000000 ) ) ;
#2215 = CARTESIAN_POINT ( 'NONE',  ( 0.07425440749237978422, 43.17733885071987032, -13.49982472904942732 ) ) ;
#2216 = CARTESIAN_POINT ( 'NONE',  ( 13.46618916530301036, 39.46328916441213863, -0.9623342693608205600 ) ) ;
#2217 = ORIENTED_EDGE ( 'NONE', *, *, #4456, .F. ) ;
#2218 = CARTESIAN_POINT ( 'NONE',  ( -4.397621424999290873, 61.33820228455973478, -12.76403019915171555 ) ) ;
#2219 = CARTESIAN_POINT ( 'NONE',  ( 2.279995255611139653E-15, 6.179999999999999716, -12.37355403259654985 ) ) ;
#2220 = VERTEX_POINT ( 'NONE', #4969 ) ;
#2221 = ORIENTED_EDGE ( 'NONE', *, *, #11736, .F. ) ;
#2222 = CARTESIAN_POINT ( 'NONE',  ( -8.343458848123576743, 31.48000000000000398, -11.48378591275254301 ) ) ;
#2223 = CARTESIAN_POINT ( 'NONE',  ( 13.16986379959834075, -14.56874999999996589, 13.16986379960055231 ) ) ;
#2224 = CARTESIAN_POINT ( 'NONE',  ( 12.04482945923018633, 48.20494489326199528, 6.111791024390479166 ) ) ;
#2225 = CARTESIAN_POINT ( 'NONE',  ( 5.704148017373132262, 57.97276112297371498, -12.24361770659877457 ) ) ;
#2226 = CARTESIAN_POINT ( 'NONE',  ( 6.299136856153257469, 78.94920042450097242, -11.94284805450234010 ) ) ;
#2227 = CARTESIAN_POINT ( 'NONE',  ( -3.636496289402155746, 78.53000000000000114, 11.19198476289190936 ) ) ;
#2228 = CARTESIAN_POINT ( 'NONE',  ( 12.74897295140808140, 2.734769208434736086E-15, -0.2137157648261680254 ) ) ;
#2229 = CARTESIAN_POINT ( 'NONE',  ( 4.206197538246464696, 6.548267719634618622, -23.28534784291399973 ) ) ;
#2230 = CARTESIAN_POINT ( 'NONE',  ( 9.744583183820527239, -100.0000000000000853, 6.703353853222205672 ) ) ;
#2231 = DIRECTION ( 'NONE',  ( 0.000000000000000000, 0.000000000000000000, -1.000000000000000000 ) ) ;
#2232 = CARTESIAN_POINT ( 'NONE',  ( 11.37499999999960565, -58.30937499999983231, 4.711679271994918317 ) ) ;
#2233 = EDGE_CURVE ( 'NONE', #12977, #5187, #10885, .T. ) ;
#2234 = CARTESIAN_POINT ( 'NONE',  ( 8.446640517145640834E-14, 43.67999999999999972, 13.50000000000000000 ) ) ;
#2235 = CARTESIAN_POINT ( 'NONE',  ( -5.485275766071775660E-07, 44.67998473833578998, 13.49999999999997691 ) ) ;
#2236 = EDGE_LOOP ( 'NONE', ( #1144, #7992, #14842, #6317 ) ) ;
#2237 = FACE_OUTER_BOUND ( 'NONE', #11787, .T. ) ;
#2238 = ORIENTED_EDGE ( 'NONE', *, *, #11600, .T. ) ;
#2239 = CARTESIAN_POINT ( 'NONE',  ( 4.171729424061791924, 16.03000000000001535, -12.83926296998457239 ) ) ;
#2240 = CARTESIAN_POINT ( 'NONE',  ( 8.043339635997654113, -85.33124999999978400, -8.043339635996304082 ) ) ;
#2241 = CARTESIAN_POINT ( 'NONE',  ( 9.615105497588862349, 78.05941236408771999, 9.479011185318192645 ) ) ;
#2242 = CARTESIAN_POINT ( 'NONE',  ( -3.928050693157006279, 59.53876161140142642, 12.91596041159252017 ) ) ;
#2243 = DIRECTION ( 'NONE',  ( 0.000000000000000000, -1.000000000000000000, 0.000000000000000000 ) ) ;
#2244 = CARTESIAN_POINT ( 'NONE',  ( -13.50000000000000000, 5.930000000000005045, -3.469446951953614189E-15 ) ) ;
#2245 = CARTESIAN_POINT ( 'NONE',  ( 13.49999999999999822, 57.27999999999998693, 4.386415899144237684 ) ) ;
#2246 = CARTESIAN_POINT ( 'NONE',  ( -3.386623526537360984, 71.55827636354801768, 13.06887847014471227 ) ) ;
#2247 = AXIS2_PLACEMENT_3D ( 'NONE', #4204, #489, #11103 ) ;
#2248 = CARTESIAN_POINT ( 'NONE',  ( 17.32050807568873552, 7.773118517290098062, 8.000000000000083489 ) ) ;
#2249 = CARTESIAN_POINT ( 'NONE',  ( 7.714727599200456254, 4.128125000000008704, -18.62499999999935341 ) ) ;
#2250 = CARTESIAN_POINT ( 'NONE',  ( -10.16858038536860498, 68.27292781118869414, 8.923254920740927076 ) ) ;
#2251 = CARTESIAN_POINT ( 'NONE',  ( 18.62500000000064304, -50.99062499999987352, -7.714727599197335195 ) ) ;
#2252 = CARTESIAN_POINT ( 'NONE',  ( 9.298704918573795553, 54.81635208236939150, -9.786940185098014666 ) ) ;
#2253 = CARTESIAN_POINT ( 'NONE',  ( 7.714727599197338748, -63.47812499999984226, 18.62500000000063949 ) ) ;
#2254 = CARTESIAN_POINT ( 'NONE',  ( -10.68045398250339417, 65.24396876513357313, 8.268639436869602122 ) ) ;
#2255 = DIRECTION ( 'NONE',  ( -1.000000000000000000, -0.000000000000000000, -2.806191565803427284E-15 ) ) ;
#2256 = CARTESIAN_POINT ( 'NONE',  ( -8.224397711408583334, 35.36732474013189886, 10.71481292070565772 ) ) ;
#2257 = CARTESIAN_POINT ( 'NONE',  ( -4.171729424061791036, 24.52999999999999758, 12.83926296998457239 ) ) ;
#2258 = VERTEX_POINT ( 'NONE', #2375 ) ;
#2259 = DIRECTION ( 'NONE',  ( 0.000000000000000000, 0.000000000000000000, -1.000000000000000000 ) ) ;
#2260 = CARTESIAN_POINT ( 'NONE',  ( 1.775737858763662015E-15, 9.000000000000000000, 14.50000000000000000 ) ) ;
#2261 = CARTESIAN_POINT ( 'NONE',  ( -12.24136337498707405, 32.13941087148443643, 5.715357471406067980 ) ) ;
#2262 = CYLINDRICAL_SURFACE ( 'NONE', #13586, 12.00000000000000178 ) ;
#2263 = CARTESIAN_POINT ( 'NONE',  ( 9.831567778977319705, 60.07019766675954742, 9.264193167865414580 ) ) ;
#2264 = CARTESIAN_POINT ( 'NONE',  ( 4.171729424061791924, -0.9699999999999986411, -12.83926296998457239 ) ) ;
#2265 = CARTESIAN_POINT ( 'NONE',  ( -6.840429191180986912, 53.42702653096863941, 11.64059165842057553 ) ) ;
#2266 = ADVANCED_FACE ( 'NONE', ( #16980, #4882 ), #3722, .F. ) ;
#2267 = CARTESIAN_POINT ( 'NONE',  ( 11.76794919243112325, 55.42999999999999972, 1.441158131103945434E-15 ) ) ;
#2268 = ITEM_DEFINED_TRANSFORMATION ( 'NONE', 'NONE', #7648,  #16654 ) ;
#2269 = CARTESIAN_POINT ( 'NONE',  ( 8.343458848123583849, 77.88000000000000966, -11.48378591275253768 ) ) ;
#2270 = CARTESIAN_POINT ( 'NONE',  ( 13.20536309241330741, 51.52922293589633540, -2.805526866140447328 ) ) ;
#2271 = CARTESIAN_POINT ( 'NONE',  ( -9.877648899171177277, 38.28753466289869323, 9.213888813852227244 ) ) ;
#2272 = CARTESIAN_POINT ( 'NONE',  ( 13.48665105718879964, 36.45067642936791685, -0.6002990102808697381 ) ) ;
#2273 = CARTESIAN_POINT ( 'NONE',  ( 11.37499999999960210, -72.80937499999984652, 4.711679271994916540 ) ) ;
#2274 = CARTESIAN_POINT ( 'NONE',  ( -0.1742961825528621111, 74.67372405737431507, 13.49999999999610623 ) ) ;
#2275 = CARTESIAN_POINT ( 'NONE',  ( -1.766402340420361483, 77.61635299055969028, 13.39115807898696353 ) ) ;
#2276 = CARTESIAN_POINT ( 'NONE',  ( -0.8900910583040317903, 80.64811563240033365, 13.47797476431978581 ) ) ;
#2277 = CARTESIAN_POINT ( 'NONE',  ( 7.500000000000000000, 108.3768542179257963, -4.091673783487169480 ) ) ;
#2278 = ORIENTED_EDGE ( 'NONE', *, *, #5501, .T. ) ;
#2279 = CARTESIAN_POINT ( 'NONE',  ( -11.76794919243112325, 9.780000000000002913, -3.823638476888998827 ) ) ;
#2280 = ORIENTED_EDGE ( 'NONE', *, *, #11024, .T. ) ;
#2281 = CARTESIAN_POINT ( 'NONE',  ( 7.272992578804311492, 55.87999999999999545, -10.01041549318726886 ) ) ;
#2282 = CARTESIAN_POINT ( 'NONE',  ( -8.043339635996302306, -6.243749999999984368, -8.043339635997654113 ) ) ;
#2283 = CARTESIAN_POINT ( 'NONE',  ( 13.50000000000000000, 56.42999999999999972, 1.653273178848926867E-15 ) ) ;
#2284 = CARTESIAN_POINT ( 'NONE',  ( 12.02097210324364518, 75.65652335936121631, -6.143864682141557232 ) ) ;
#2285 = CARTESIAN_POINT ( 'NONE',  ( -1.564113515457998572E-12, -29.13749999999993179, 18.62500000000000000 ) ) ;
#2286 = CARTESIAN_POINT ( 'NONE',  ( -10.92172942406178926, 73.62999999999999545, -7.935100905948389460 ) ) ;
#2287 = EDGE_CURVE ( 'NONE', #5098, #6231, #2807, .T. ) ;
#2288 = CARTESIAN_POINT ( 'NONE',  ( -7.272992578804307939, 47.47999999999998977, -10.01041549318726886 ) ) ;
#2289 = DIRECTION ( 'NONE',  ( 0.000000000000000000, -1.000000000000000000, 0.000000000000000000 ) ) ;
#2290 = CARTESIAN_POINT ( 'NONE',  ( -13.43445895775833598, 58.88303016948394486, -1.354977829824218771 ) ) ;
#2291 = CARTESIAN_POINT ( 'NONE',  ( 10.43514330751975194, 45.10252430648384347, 8.564926864381755323 ) ) ;
#2292 = CARTESIAN_POINT ( 'NONE',  ( 13.10873240010329077, 69.54468864661862426, -3.226680269542550050 ) ) ;
#2293 = VECTOR ( 'NONE', #9477, 1000.000000000000000 ) ;
#2294 = LINE ( 'NONE', #16984, #4983 ) ;
#2295 = CARTESIAN_POINT ( 'NONE',  ( 12.02303304563724673, 30.65636901295595607, -6.139761926991930352 ) ) ;
#2296 = CARTESIAN_POINT ( 'NONE',  ( -7.135146516150340901, 55.44532162981700907, -11.46164669714722528 ) ) ;
#2297 = CARTESIAN_POINT ( 'NONE',  ( -13.24244078534688818, 50.02386753338626590, 2.657835324058360094 ) ) ;
#2298 = CARTESIAN_POINT ( 'NONE',  ( 7.466952291864066282, 63.90051593161832955, -11.24819315821802768 ) ) ;
#2299 = CARTESIAN_POINT ( 'NONE',  ( 12.99392763564549291, 42.56084116897148562, -3.661734528280473189 ) ) ;
#2300 = CARTESIAN_POINT ( 'NONE',  ( 13.43182422821157118, 39.38122741038952768, 1.395845098213416957 ) ) ;
#2301 = ORIENTED_EDGE ( 'NONE', *, *, #9840, .T. ) ;
#2302 = CARTESIAN_POINT ( 'NONE',  ( -7.631036692897547269, 70.46660093273136738, -11.13720947216162216 ) ) ;
#2303 = CARTESIAN_POINT ( 'NONE',  ( -12.16104664928658963, 61.71474001778207708, -5.861914737776502626 ) ) ;
#2304 = CARTESIAN_POINT ( 'NONE',  ( 3.636496289402157078, 9.030000000000010019, -11.19198476289190936 ) ) ;
#2305 = ORIENTED_EDGE ( 'NONE', *, *, #4294, .F. ) ;
#2306 = CARTESIAN_POINT ( 'NONE',  ( -12.71421417626428152, 40.76452965150037500, -4.584416513558855932 ) ) ;
#2307 = EDGE_LOOP ( 'NONE', ( #15806, #11981, #15306, #5419 ) ) ;
#2308 = CARTESIAN_POINT ( 'NONE',  ( -10.92172942406179104, 26.23000000000000398, 7.935100905948385908 ) ) ;
#2309 = CARTESIAN_POINT ( 'NONE',  ( -13.16986379959834252, -96.74374999999980673, -13.16986379960055409 ) ) ;
#2310 = CARTESIAN_POINT ( 'NONE',  ( 3.942382125243764524, 47.82151681360642215, 12.91477671872532618 ) ) ;
#2311 = AXIS2_PLACEMENT_3D ( 'NONE', #2914, #13700, #13872 ) ;
#2312 = CARTESIAN_POINT ( 'NONE',  ( 10.52817469841624387, 57.75233781933106059, -8.450342176037976216 ) ) ;
#2313 = CARTESIAN_POINT ( 'NONE',  ( 12.19096715004470788, 78.64285588553632067, -5.799165764274725632 ) ) ;
#2314 = CARTESIAN_POINT ( 'NONE',  ( -11.76794919243112325, 81.07999999999998408, 3.823638476888994386 ) ) ;
#2315 = CARTESIAN_POINT ( 'NONE',  ( 12.71634493074430594, -4.622062490413149683E-15, 2.191283809529018356 ) ) ;
#2316 = EDGE_CURVE ( 'NONE', #11794, #717, #890, .T. ) ;
#2317 = CARTESIAN_POINT ( 'NONE',  ( 2.970370385949292036, 7.170662809914417402, -21.14483242576214650 ) ) ;
#2318 = CARTESIAN_POINT ( 'NONE',  ( 8.833428499591450489, -99.99999999999995737, 8.182135825729266898 ) ) ;
#2319 = CARTESIAN_POINT ( 'NONE',  ( 2.445080149700053643E-15, 75.17999999999999261, -13.50000000000000000 ) ) ;
#2320 = CARTESIAN_POINT ( 'NONE',  ( 4.711679271994909435, -19.77187499999995168, -11.37499999999960387 ) ) ;
#2321 = VECTOR ( 'NONE', #780, 1000.000000000000000 ) ;
#2322 = CARTESIAN_POINT ( 'NONE',  ( 1.469576158976824144E-15, 0.000000000000000000, -12.00000000000000178 ) ) ;
#2323 = CARTESIAN_POINT ( 'NONE',  ( 6.429988302422167123, 33.94387318707013890, -11.87465190390881453 ) ) ;
#2324 = CARTESIAN_POINT ( 'NONE',  ( -12.44080865564263583, 73.73893818206965989, -5.243278813652959336 ) ) ;
#2325 = VERTEX_POINT ( 'NONE', #17241 ) ;
#2326 = VERTEX_POINT ( 'NONE', #13349 ) ;
#2327 = DIRECTION ( 'NONE',  ( 0.000000000000000000, 0.000000000000000000, -1.000000000000000000 ) ) ;
#2328 = VERTEX_POINT ( 'NONE', #9048 ) ;
#2329 = CARTESIAN_POINT ( 'NONE',  ( -11.37499999999960210, -47.83437499999990195, -4.711679271994911211 ) ) ;
#2330 = CARTESIAN_POINT ( 'NONE',  ( -8.356910137473439804, 59.36152714647494832, 10.62299724927810729 ) ) ;
#2331 = CARTESIAN_POINT ( 'NONE',  ( -17.32050807568867512, 0.000000000000000000, -8.000000000000207834 ) ) ;
#2332 = CARTESIAN_POINT ( 'NONE',  ( -19.29752010712865129, 5.918584287042170544, 17.42428528562837542 ) ) ;
#2333 = CARTESIAN_POINT ( 'NONE',  ( 4.171729424061789260, 53.83000000000000540, 12.83926296998457417 ) ) ;
#2334 = CARTESIAN_POINT ( 'NONE',  ( -5.941256636048077411, 71.46338852619901161, 12.12314389860511277 ) ) ;
#2335 = ADVANCED_FACE ( 'NONE', ( #8961 ), #6302, .T. ) ;
#2336 = APPLICATION_CONTEXT ( 'automotive_design' ) ;
#2337 = CARTESIAN_POINT ( 'NONE',  ( 18.62500000000000000, -66.59999999999983800, 1.560692158462880521E-12 ) ) ;
#2338 = CARTESIAN_POINT ( 'NONE',  ( -4.083439365806073695, 68.53322352374333093, 12.86826179363684197 ) ) ;
#2339 = CARTESIAN_POINT ( 'NONE',  ( -7.714727599197335195, -21.85312499999995239, -18.62500000000064304 ) ) ;
#2340 = CARTESIAN_POINT ( 'NONE',  ( 9.456157084575252725, 54.80849625928562574, -9.635361094816037308 ) ) ;
#2341 = CARTESIAN_POINT ( 'NONE',  ( -7.272992578804307939, 18.48000000000000398, -10.01041549318726886 ) ) ;
#2342 = CARTESIAN_POINT ( 'NONE',  ( -18.62499999999934985, -57.23437499999987921, -7.714727599200458918 ) ) ;
#2343 = CARTESIAN_POINT ( 'NONE',  ( -9.809219749064693517, 65.29068444701793794, 9.275196495002377972 ) ) ;
#2344 = CARTESIAN_POINT ( 'NONE',  ( 10.68680102524458242, 7.855179386613375669, -15.43414541437280185 ) ) ;
#2345 = CARTESIAN_POINT ( 'NONE',  ( -7.048305978417979567, 35.41831309511212567, 11.51397633767918904 ) ) ;
#2346 = CARTESIAN_POINT ( 'NONE',  ( 8.343458848123583849, 19.87999999999999901, -11.48378591275253768 ) ) ;
#2347 = ORIENTED_EDGE ( 'NONE', *, *, #3035, .T. ) ;
#2348 = CARTESIAN_POINT ( 'NONE',  ( 13.50000000000000355, 50.58000000000000540, -4.386415899144233244 ) ) ;
#2349 = CARTESIAN_POINT ( 'NONE',  ( -4.132008100336891587, 40.32855870418434563, -12.85265726257471108 ) ) ;
#2350 = CARTESIAN_POINT ( 'NONE',  ( -13.25105815227180805, 32.02163500762459591, 2.596925824824028339 ) ) ;
#2351 = CARTESIAN_POINT ( 'NONE',  ( 0.5158602612934328757, 73.16145157157426127, -13.49014129109500360 ) ) ;
#2352 = CARTESIAN_POINT ( 'NONE',  ( 11.66024569017766410, 60.17689946827382386, 6.803589074568463957 ) ) ;
#2353 = CARTESIAN_POINT ( 'NONE',  ( -4.171729424061787483, -6.669999999999995488, -12.83926296998457417 ) ) ;
#2354 = CARTESIAN_POINT ( 'NONE',  ( -2.138718998850744679, 53.60317316735872595, 13.33842984004382970 ) ) ;
#2355 = CARTESIAN_POINT ( 'NONE',  ( 3.636496289402154414, 54.83000000000000540, 11.19198476289190936 ) ) ;
#2356 = CARTESIAN_POINT ( 'NONE',  ( 8.343458848123583849, 74.88000000000000966, -11.48378591275253768 ) ) ;
#2357 = CARTESIAN_POINT ( 'NONE',  ( 11.09074627470785401, 51.72008494892603636, -7.700087750201487502 ) ) ;
#2358 = CARTESIAN_POINT ( 'NONE',  ( -12.57349182499318019, 38.10837077157162867, 4.915015114056598300 ) ) ;
#2359 = CARTESIAN_POINT ( 'NONE',  ( 13.48517604768645661, 36.45179642338925419, -0.6325697479206738860 ) ) ;
#2360 = CARTESIAN_POINT ( 'NONE',  ( -11.37499999999999645, -48.87499999999990052, -9.545674412382054647E-13 ) ) ;
#2361 = CARTESIAN_POINT ( 'NONE',  ( 1.900613283894437622, 2.969143981464173798, -12.00000000000000000 ) ) ;
#2362 = CARTESIAN_POINT ( 'NONE',  ( -3.925525489409863233, 77.53884384066057578, 12.91671140569806830 ) ) ;
#2363 = CARTESIAN_POINT ( 'NONE',  ( -7.076833851983480805, 80.41718626680707871, 11.49927917534153110 ) ) ;
#2364 = CARTESIAN_POINT ( 'NONE',  ( 7.500000000000001776, 107.4971863040494497, -6.484415072061725738 ) ) ;
#2365 = EDGE_LOOP ( 'NONE', ( #13383, #9938, #16647, #3030 ) ) ;
#2366 = CARTESIAN_POINT ( 'NONE',  ( -7.409984580736203970E-16, 10.68000000000000149, 12.37355403259654985 ) ) ;
#2367 = EDGE_CURVE ( 'NONE', #1772, #4303, #3544, .T. ) ;
#2368 = ORIENTED_EDGE ( 'NONE', *, *, #13434, .T. ) ;
#2369 = CARTESIAN_POINT ( 'NONE',  ( 11.76794919243112325, 61.42999999999999972, 1.441158131103945434E-15 ) ) ;
#2370 = CARTESIAN_POINT ( 'NONE',  ( -8.043339635997654113, -86.40624999999977263, 8.043339635996304082 ) ) ;
#2371 = CARTESIAN_POINT ( 'NONE',  ( 10.55733521878493697, 75.75071791524901244, -8.413839998617302030 ) ) ;
#2372 = CYLINDRICAL_SURFACE ( 'NONE', #11067, 13.50000000000000000 ) ;
#2373 = CARTESIAN_POINT ( 'NONE',  ( -4.171729424061791036, 71.53000000000000114, 12.83926296998457239 ) ) ;
#2374 = CARTESIAN_POINT ( 'NONE',  ( 11.76794919243112325, 40.42999999999999972, 1.441158131103945434E-15 ) ) ;
#2375 = CARTESIAN_POINT ( 'NONE',  ( 2.222800136090958861E-15, 3.313974596215566670, -12.00000000000000355 ) ) ;
#2376 = CARTESIAN_POINT ( 'NONE',  ( -10.14977031755370263, 59.27292367458827727, 8.902714087877939164 ) ) ;
#2377 = CARTESIAN_POINT ( 'NONE',  ( 13.41602063970378289, 45.49023818299943400, -1.729735045551601402 ) ) ;
#2378 = CARTESIAN_POINT ( 'NONE',  ( 13.41279318566184209, 69.49145390545891132, -1.766636264389374489 ) ) ;
#2379 = CARTESIAN_POINT ( 'NONE',  ( 6.173563035904286345, 80.90543369209835589, 12.02534506568683170 ) ) ;
#2380 = CARTESIAN_POINT ( 'NONE',  ( 11.66233170971271704, 30.17662848724782521, 6.809971670536899779 ) ) ;
#2381 = CARTESIAN_POINT ( 'NONE',  ( -9.573451043744061195, 55.55711678553799970, -9.523417059222403225 ) ) ;
#2382 = CARTESIAN_POINT ( 'NONE',  ( -13.48277841417289302, 49.90646545391939526, -0.6818155833736215810 ) ) ;
#2383 = CARTESIAN_POINT ( 'NONE',  ( 18.99999999999999289, 7.773118517290098062, 1.732050807568941586 ) ) ;
#2384 = CARTESIAN_POINT ( 'NONE',  ( 10.17565235674593005, 42.77150727048867651, -8.872034920332040997 ) ) ;
#2385 = CARTESIAN_POINT ( 'NONE',  ( 11.19208411514268420, 39.14620708772159219, 7.549024317084779057 ) ) ;
#2386 = VERTEX_POINT ( 'NONE', #11688 ) ;
#2387 = CARTESIAN_POINT ( 'NONE',  ( -12.72731565556658673, 70.76746085843132050, -4.502049236143019328 ) ) ;
#2388 = CARTESIAN_POINT ( 'NONE',  ( -10.21469213217646121, 61.59053157756512320, -8.827045802700096644 ) ) ;
#2389 =( BOUNDED_CURVE ( )  B_SPLINE_CURVE ( 2, ( #4661, #8740, #3232, #14006, #14098, #7060, #9717, #5736, #15153, #15418, #10068, #11289, #3325 ),
 .UNSPECIFIED., .F., .F. ) 
 B_SPLINE_CURVE_WITH_KNOTS ( ( 3, 2, 2, 2, 2, 2, 3 ),
 ( 0.6805555555555555802, 0.6833333333333333481, 0.6888888888888888840, 0.6944444444444444198, 0.6999999999999999556, 0.7055555555555556024, 0.7083333333333333703 ),
 .UNSPECIFIED. ) 
 CURVE ( )  GEOMETRIC_REPRESENTATION_ITEM ( )  RATIONAL_B_SPLINE_CURVE ( ( 0.9755282581475768211, 0.9755282581475768211, 1.000000000000000000, 0.9510565162951535312, 1.000000000000000000, 0.9510565162951535312, 1.000000000000000000, 0.9510565162951535312, 1.000000000000000000, 0.9510565162951535312, 1.000000000000000000, 0.9755282581475768211, 0.9755282581475768211 ) ) 
 REPRESENTATION_ITEM ( '' )  );
#2390 = CARTESIAN_POINT ( 'NONE',  ( -9.520470885617715595, 3.629999999999994564, -6.917026985038136289 ) ) ;
#2391 = EDGE_LOOP ( 'NONE', ( #13742, #12043, #3122, #7756 ) ) ;
#2392 = VERTEX_POINT ( 'NONE', #9312 ) ;
#2393 = CARTESIAN_POINT ( 'NONE',  ( 4.171729424061791924, 22.02999999999999403, -12.83926296998457239 ) ) ;
#2394 = CARTESIAN_POINT ( 'NONE',  ( 13.16986379959834075, -97.81874999999976694, 13.16986379960055231 ) ) ;
#2395 = VECTOR ( 'NONE', #8790, 1000.000000000000227 ) ;
#2396 = CARTESIAN_POINT ( 'NONE',  ( 13.37052541849207188, 57.49521496994567826, -1.865347435624440164 ) ) ;
#2397 = CARTESIAN_POINT ( 'NONE',  ( -11.76794919243112325, 71.92999999999999261, -2.882316262207890869E-15 ) ) ;
#2398 = CARTESIAN_POINT ( 'NONE',  ( 7.272992578804311492, 79.87999999999999545, -10.01041549318726709 ) ) ;
#2399 = CARTESIAN_POINT ( 'NONE',  ( 8.343458848123580296, 0.9799999999999967626, 11.48378591275253768 ) ) ;
#2400 = CARTESIAN_POINT ( 'NONE',  ( -1.732050807569007977, 7.773118517290099838, 18.99999999999998224 ) ) ;
#2401 = CARTESIAN_POINT ( 'NONE',  ( 4.988803385412796665, 9.999999999999996447, -12.54439479535357371 ) ) ;
#2402 = CARTESIAN_POINT ( 'NONE',  ( -8.043339635997654113, -10.40624999999997513, 8.043339635996302306 ) ) ;
#2403 = DIRECTION ( 'NONE',  ( -1.000000000000000000, -0.000000000000000000, -0.000000000000000000 ) ) ;
#2404 = DIRECTION ( 'NONE',  ( 0.000000000000000000, -1.000000000000000000, 0.000000000000000000 ) ) ;
#2405 = CARTESIAN_POINT ( 'NONE',  ( -7.982953728650207026, 73.48208634606795897, -10.88794980213214103 ) ) ;
#2406 = ORIENTED_EDGE ( 'NONE', *, *, #10160, .T. ) ;
#2407 = EDGE_CURVE ( 'NONE', #3478, #14678, #6480, .T. ) ;
#2408 = ORIENTED_EDGE ( 'NONE', *, *, #9356, .F. ) ;
#2409 = CARTESIAN_POINT ( 'NONE',  ( -11.76794919243112325, 74.78000000000000114, -3.823638476888998827 ) ) ;
#2410 = ORIENTED_EDGE ( 'NONE', *, *, #10270, .T. ) ;
#2411 = CARTESIAN_POINT ( 'NONE',  ( 13.50000000000000000, 12.42999999999999616, 1.734723475976807094E-15 ) ) ;
#2412 = CARTESIAN_POINT ( 'NONE',  ( 8.043339635996298753, -71.76874999999985505, 8.043339635997652337 ) ) ;
#2413 = CARTESIAN_POINT ( 'NONE',  ( -7.479440193669519843, 44.39995570584004980, 11.23875935782371371 ) ) ;
#2414 = CARTESIAN_POINT ( 'NONE',  ( -7.499999999999995559, -24.66999453389980346, -8.557281619885989343 ) ) ;
#2415 = CARTESIAN_POINT ( 'NONE',  ( 10.12510679658022461, 66.77424677226939309, -8.932337163854400686 ) ) ;
#2416 = CARTESIAN_POINT ( 'NONE',  ( 8.343458848123583849, 51.87999999999999545, -11.48378591275253768 ) ) ;
#2417 = CARTESIAN_POINT ( 'NONE',  ( -5.514649017516719098, 71.48002869512200164, 12.32322048284371263 ) ) ;
#2418 = CARTESIAN_POINT ( 'NONE',  ( 1.561832610794586538E-12, -87.41249999999979536, -18.62500000000000000 ) ) ;
#2419 = CARTESIAN_POINT ( 'NONE',  ( -12.85543916597470115, 68.07811659554265304, 4.121900813656875329 ) ) ;
#2420 = CARTESIAN_POINT ( 'NONE',  ( 7.714727599200456254, 4.128125000000008704, -18.62499999999935341 ) ) ;
#2421 = CARTESIAN_POINT ( 'NONE',  ( 4.683651263586128266, 55.01126310294681332, -12.66170012766897557 ) ) ;
#2422 = CARTESIAN_POINT ( 'NONE',  ( 9.520470885617715595, 20.13000000000000966, 6.917026985038135400 ) ) ;
#2423 = CARTESIAN_POINT ( 'NONE',  ( 13.16986379959834075, -31.21874999999992539, 13.16986379960055231 ) ) ;
#2424 = AXIS2_PLACEMENT_3D ( 'NONE', #10229, #3318, #15585 ) ;
#2425 = CARTESIAN_POINT ( 'NONE',  ( -7.387617763983256758, 65.40391021994592791, 11.29955664239258084 ) ) ;
#2426 = EDGE_CURVE ( 'NONE', #6499, #967, #11775, .T. ) ;
#2427 = CARTESIAN_POINT ( 'NONE',  ( 8.446640517145640834E-14, 43.67999999999999972, 13.50000000000000000 ) ) ;
#2428 = CARTESIAN_POINT ( 'NONE',  ( -11.39564835574532964, 35.20092729567576839, 7.239028663105881556 ) ) ;
#2429 = CARTESIAN_POINT ( 'NONE',  ( 13.49999999999999822, 22.28000000000000469, 4.386415899144237684 ) ) ;
#2430 = EDGE_LOOP ( 'NONE', ( #10834, #17171, #4568, #16470, #13280, #10923, #13875, #2192 ) ) ;
#2431 = CARTESIAN_POINT ( 'NONE',  ( -4.171729424061787483, 8.330000000000003624, -12.83926296998457417 ) ) ;
#2432 = CARTESIAN_POINT ( 'NONE',  ( -11.76794919243112325, 33.78000000000000824, -3.823638476888998827 ) ) ;
#2433 = CARTESIAN_POINT ( 'NONE',  ( -13.31326865110370328, 32.00865534729634021, 2.238786097854670754 ) ) ;
#2434 = FACE_OUTER_BOUND ( 'NONE', #6319, .T. ) ;
#2435 = CARTESIAN_POINT ( 'NONE',  ( 7.029870786644410785, 59.94104792918457747, 11.52738832307962369 ) ) ;
#2436 = CARTESIAN_POINT ( 'NONE',  ( -7.696137532356187805, 53.39059926922609378, 11.09266641989247049 ) ) ;
#2437 = CARTESIAN_POINT ( 'NONE',  ( -7.272992578804307939, 53.47999999999998977, -10.01041549318726886 ) ) ;
#2438 = CARTESIAN_POINT ( 'NONE',  ( 8.343458848123583849, 71.87999999999998124, -11.48378591275253768 ) ) ;
#2439 = CARTESIAN_POINT ( 'NONE',  ( 9.077726944796655317, 51.03253575000494635, 10.00638466558158512 ) ) ;
#2440 = CARTESIAN_POINT ( 'NONE',  ( -11.71421975593653997, 37.68063548265865137, -6.711783420003171408 ) ) ;
#2441 = CARTESIAN_POINT ( 'NONE',  ( 2.303310151039730247, 35.76279920576850913, 13.30420860107493652 ) ) ;
#2442 = CARTESIAN_POINT ( 'NONE',  ( -11.37499999999999645, -15.57499999999997975, -9.545674412382054647E-13 ) ) ;
#2443 = CARTESIAN_POINT ( 'NONE',  ( -3.216530273324876621, 74.56434933806751530, 13.11174169623774333 ) ) ;
#2444 = B_SPLINE_CURVE_WITH_KNOTS ( 'NONE', 3,
 ( #15986, #4154, #9566, #181 ),
 .UNSPECIFIED., .F., .F.,
 ( 4, 4 ),
 ( 0.000000000000000000, 1.000000000000000000 ),
 .UNSPECIFIED. ) ;
#2445 = CARTESIAN_POINT ( 'NONE',  ( -6.363446314678021132, 77.44652370057923463, 11.90615704593929536 ) ) ;
#2446 = ADVANCED_FACE ( 'NONE', ( #10542 ), #15904, .F. ) ;
#2447 = CARTESIAN_POINT ( 'NONE',  ( -13.49462269136053827, 79.94511885973835774, 0.4405215047912745541 ) ) ;
#2448 = CARTESIAN_POINT ( 'NONE',  ( -1.328659818498353332E-07, 59.67999629905246195, 13.49999999999999822 ) ) ;
#2449 = ORIENTED_EDGE ( 'NONE', *, *, #3081, .T. ) ;
#2450 = CARTESIAN_POINT ( 'NONE',  ( 0.000000000000000000, 80.93000000000000682, -13.50000000000000000 ) ) ;
#2451 = CARTESIAN_POINT ( 'NONE',  ( -11.76794919243112325, 7.080000000000000959, 3.823638476888994386 ) ) ;
#2452 = EDGE_LOOP ( 'NONE', ( #2066, #15743, #16906, #8909, #878, #5361 ) ) ;
#2453 = CARTESIAN_POINT ( 'NONE',  ( -11.76794919243112325, 54.07999999999999829, 3.823638476888994830 ) ) ;
#2454 = CARTESIAN_POINT ( 'NONE',  ( -11.37500000000039790, -85.36562499999978115, 4.711679271993001628 ) ) ;
#2455 = DIRECTION ( 'NONE',  ( 0.000000000000000000, 0.000000000000000000, 1.000000000000000000 ) ) ;
#2456 = CARTESIAN_POINT ( 'NONE',  ( 13.50000000000000355, -8.420000000000003482, -4.386415899144233244 ) ) ;
#2457 = CARTESIAN_POINT ( 'NONE',  ( 9.024310119946591158, 75.82999935558571281, -10.05502432205268626 ) ) ;
#2458 = FACE_OUTER_BOUND ( 'NONE', #12783, .T. ) ;
#2459 = CARTESIAN_POINT ( 'NONE',  ( 10.92172942406178926, 69.12999999999999545, 7.935100905948387684 ) ) ;
#2460 = CARTESIAN_POINT ( 'NONE',  ( 11.76794919243112325, 37.42999999999999972, 1.441158131103945434E-15 ) ) ;
#2461 = CARTESIAN_POINT ( 'NONE',  ( 0.000000000000000000, -22.00000000000000000, 0.000000000000000000 ) ) ;
#2462 = CARTESIAN_POINT ( 'NONE',  ( -12.57014003203463304, 58.75104985464606955, -4.931354137584416542 ) ) ;
#2463 = CARTESIAN_POINT ( 'NONE',  ( 6.882857235644580740, 44.93490147452389039, 11.61738766344687868 ) ) ;
#2464 = CARTESIAN_POINT ( 'NONE',  ( 11.94122772029547619, 69.66266832655985297, -6.297391191416378931 ) ) ;
#2465 = CARTESIAN_POINT ( 'NONE',  ( -4.171729424061787483, 66.32999999999999829, -12.83926296998457417 ) ) ;
#2466 = CARTESIAN_POINT ( 'NONE',  ( -15.58845726811999910, 0.000000000000000000, 10.99999999999985256 ) ) ;
#2467 = CARTESIAN_POINT ( 'NONE',  ( -3.638089963872648269, 55.31079992990586192, -13.00509624865515690 ) ) ;
#2468 = CARTESIAN_POINT ( 'NONE',  ( -11.02862702592511290, 50.22370839642280060, 7.785847849197222281 ) ) ;
#2469 = CARTESIAN_POINT ( 'NONE',  ( 12.90275692282559028, 63.28756754940194185, 3.971062145897854556 ) ) ;
#2470 = CARTESIAN_POINT ( 'NONE',  ( 11.93121478369607402, 42.66342760203531270, -6.316342296523080435 ) ) ;
#2471 = CARTESIAN_POINT ( 'NONE',  ( 9.269155314290372871, 39.04219773109588232, 9.814949453710875460 ) ) ;
#2472 = VERTEX_POINT ( 'NONE', #9226 ) ;
#2473 = CARTESIAN_POINT ( 'NONE',  ( -13.31540386738444681, 70.85153878471251687, -2.233583993245589649 ) ) ;
#2474 = CARTESIAN_POINT ( 'NONE',  ( -4.261210048699548558, 61.33323415936689571, -12.81044948870924394 ) ) ;
#2475 = CARTESIAN_POINT ( 'NONE',  ( -3.636496289402156190, 1.530000000000003579, 11.19198476289190758 ) ) ;
#2476 = ORIENTED_EDGE ( 'NONE', *, *, #14586, .F. ) ;
#2477 = ORIENTED_EDGE ( 'NONE', *, *, #4272, .T. ) ;
#2478 = CARTESIAN_POINT ( 'NONE',  ( -8.549982208541774191E-16, 20.68000000000001037, 14.19474002721660355 ) ) ;
#2479 = CARTESIAN_POINT ( 'NONE',  ( -18.62499999999934985, -73.88437499999982094, -7.714727599200458918 ) ) ;
#2480 = CARTESIAN_POINT ( 'NONE',  ( 5.076768451170277530, 47.86330475330473178, 12.50906521756310141 ) ) ;
#2481 = CARTESIAN_POINT ( 'NONE',  ( 10.64294614749145573, 72.11408737100931887, 8.305316784397419383 ) ) ;
#2482 = CARTESIAN_POINT ( 'NONE',  ( 13.41154217937975446, 57.37612970769495746, 1.546557898521643937 ) ) ;
#2483 = CARTESIAN_POINT ( 'NONE',  ( -3.636496289402155746, 66.53000000000000114, 11.19198476289190936 ) ) ;
#2484 = CARTESIAN_POINT ( 'NONE',  ( -11.76794919243112325, 75.08000000000001251, 3.823638476888994386 ) ) ;
#2485 = CARTESIAN_POINT ( 'NONE',  ( -1.150288393095961981, 47.63866982340532985, 13.45354997221035909 ) ) ;
#2486 = CIRCLE ( 'NONE', #12391, 1.999999999999998224 ) ;
#2487 = EDGE_CURVE ( 'NONE', #2386, #16561, #4685, .T. ) ;
#2488 = CARTESIAN_POINT ( 'NONE',  ( 2.138189944381238661, 37.75688142232025513, 13.50000000000000000 ) ) ;
#2489 = CARTESIAN_POINT ( 'NONE',  ( -13.50000000000000000, 75.92999999999999261, -3.306546357697853733E-15 ) ) ;
#2490 = CARTESIAN_POINT ( 'NONE',  ( 11.37500000000000000, -33.29999999999991900, 9.531744055041752924E-13 ) ) ;
#2491 =( BOUNDED_CURVE ( )  B_SPLINE_CURVE ( 2, ( #9497, #10896, #14844, #16088, #17, #13531, #15023, #108, #16265, #3996, #2738, #4172, #14760 ),
 .UNSPECIFIED., .F., .F. ) 
 B_SPLINE_CURVE_WITH_KNOTS ( ( 3, 2, 2, 2, 2, 2, 3 ),
 ( 0.6527777777777777901, 0.6555555555555555580, 0.6611111111111110938, 0.6666666666666666297, 0.6722222222222222765, 0.6777777777777778123, 0.6805555555555555802 ),
 .UNSPECIFIED. ) 
 CURVE ( )  GEOMETRIC_REPRESENTATION_ITEM ( )  RATIONAL_B_SPLINE_CURVE ( ( 0.9755282581475768211, 0.9755282581475768211, 1.000000000000000000, 0.9510565162951535312, 1.000000000000000000, 0.9510565162951535312, 1.000000000000000000, 0.9510565162951535312, 1.000000000000000000, 0.9510565162951535312, 1.000000000000000000, 0.9755282581475768211, 0.9755282581475768211 ) ) 
 REPRESENTATION_ITEM ( '' )  );
#2492 = FACE_OUTER_BOUND ( 'NONE', #6519, .T. ) ;
#2493 = CARTESIAN_POINT ( 'NONE',  ( 9.964133567250449630, 33.78271751155136116, -9.110518748047969240 ) ) ;
#2494 = CARTESIAN_POINT ( 'NONE',  ( -9.651932366745469949, 73.56128327655086707, -9.438761847476623501 ) ) ;
#2495 = ORIENTED_EDGE ( 'NONE', *, *, #5631, .F. ) ;
#2496 = ORIENTED_EDGE ( 'NONE', *, *, #12815, .F. ) ;
#2497 = CARTESIAN_POINT ( 'NONE',  ( 7.272992578804311492, 73.87999999999999545, -10.01041549318726886 ) ) ;
#2498 = ORIENTED_EDGE ( 'NONE', *, *, #319, .T. ) ;
#2499 = CARTESIAN_POINT ( 'NONE',  ( -3.636496289402152637, -11.66999999999999993, -11.19198476289190936 ) ) ;
#2500 = CARTESIAN_POINT ( 'NONE',  ( -9.552639591052204498E-13, -69.68749999999984368, 11.37499999999999645 ) ) ;
#2501 = CIRCLE ( 'NONE', #557, 4.000000000000004441 ) ;
#2502 = CARTESIAN_POINT ( 'NONE',  ( -7.379967326026998009, 44.40423310405564905, 11.30426345811079258 ) ) ;
#2503 = CARTESIAN_POINT ( 'NONE',  ( -7.499999999999996447, -23.02360215807748745, -9.261711852864912942 ) ) ;
#2504 = CARTESIAN_POINT ( 'NONE',  ( 13.40272165065616150, 66.48640177007516172, -1.617736196660548575 ) ) ;
#2505 = CARTESIAN_POINT ( 'NONE',  ( 13.49999999999999822, 48.27999999999998693, 4.386415899144237684 ) ) ;
#2506 = CARTESIAN_POINT ( 'NONE',  ( -8.178477986879377326, 71.36909458440034371, 10.74071161083785420 ) ) ;
#2507 = EDGE_CURVE ( 'NONE', #16109, #6836, #11947, .T. ) ;
#2508 = CARTESIAN_POINT ( 'NONE',  ( -1.564113515457998572E-12, -95.73749999999976978, 18.62500000000000000 ) ) ;
#2509 = CARTESIAN_POINT ( 'NONE',  ( -13.50000235157018480, 67.93091628171310958, 0.02679276516280407541 ) ) ;
#2510 = CARTESIAN_POINT ( 'NONE',  ( 13.16986379959833897, -23.96874999999992539, 13.16986379960055409 ) ) ;
#2511 = CARTESIAN_POINT ( 'NONE',  ( 4.849954924687469138, 55.00518118710664339, -12.59872946003133620 ) ) ;
#2512 = CARTESIAN_POINT ( 'NONE',  ( 9.520470885617715595, 17.13000000000000611, 6.917026985038135400 ) ) ;
#2513 = CARTESIAN_POINT ( 'NONE',  ( 7.714727599197338748, -96.77812499999976126, 18.62500000000063949 ) ) ;
#2514 = CARTESIAN_POINT ( 'NONE',  ( -13.21884357211656180, 65.02777525366441580, 2.766200456887108583 ) ) ;
#2515 = CARTESIAN_POINT ( 'NONE',  ( -8.992723398997755524, 35.33141607309799070, 10.07310997216105974 ) ) ;
#2516 = CARTESIAN_POINT ( 'NONE',  ( 4.171729424061791924, 20.02999999999999403, -12.83926296998457239 ) ) ;
#2517 = ORIENTED_EDGE ( 'NONE', *, *, #2212, .F. ) ;
#2518 = DIRECTION ( 'NONE',  ( 0.000000000000000000, 0.000000000000000000, -1.000000000000000000 ) ) ;
#2519 = CARTESIAN_POINT ( 'NONE',  ( -15.58845726811976817, 0.000000000000000000, -11.00000000000018296 ) ) ;
#2520 = CARTESIAN_POINT ( 'NONE',  ( -11.76794919243112325, 28.08000000000000540, 3.823638476888994386 ) ) ;
#2521 = CARTESIAN_POINT ( 'NONE',  ( -2.757445517627192810, 31.27914755613021924, -13.21542082288816289 ) ) ;
#2522 = CARTESIAN_POINT ( 'NONE',  ( -3.320475467054404886E-07, 70.18000001193918536, -13.49999999999999467 ) ) ;
#2523 = CARTESIAN_POINT ( 'NONE',  ( -11.76794919243112325, -8.220000000000004192, -3.823638476888998827 ) ) ;
#2524 = CARTESIAN_POINT ( 'NONE',  ( 11.65227599590961027, 60.17634486657772186, 6.817218417200347602 ) ) ;
#2525 = CARTESIAN_POINT ( 'NONE',  ( -13.49999999999999822, -8.920000000000001705, 4.386415899144235908 ) ) ;
#2526 = CARTESIAN_POINT ( 'NONE',  ( -3.961000965835436816, 53.53757305567045677, 12.90588582463717060 ) ) ;
#2527 = CARTESIAN_POINT ( 'NONE',  ( 7.272992578804311492, 52.87999999999998835, -10.01041549318726709 ) ) ;
#2528 = APPLICATION_PROTOCOL_DEFINITION ( 'draft international standard', 'automotive_design', 1998, #2336 ) ;
#2529 = CARTESIAN_POINT ( 'NONE',  ( -13.49999999999999822, 70.08000000000001251, 4.386415899144235908 ) ) ;
#2530 = EDGE_CURVE ( 'NONE', #3828, #4826, #7231, .T. ) ;
#2531 = CARTESIAN_POINT ( 'NONE',  ( 13.22222055999062462, 51.33170938898963698, 2.778060537294016363 ) ) ;
#2532 = CARTESIAN_POINT ( 'NONE',  ( -11.86684622039495274, 37.69174919575652183, -6.436470158516030438 ) ) ;
#2533 = CARTESIAN_POINT ( 'NONE',  ( 13.43970656773339201, 36.38377728058151206, 1.324025325594676783 ) ) ;
#2534 = CARTESIAN_POINT ( 'NONE',  ( -11.37499999999999645, -98.82499999999978968, -9.545674412382054647E-13 ) ) ;
#2535 = CARTESIAN_POINT ( 'NONE',  ( 12.00000000000000178, 2.296025403784453189, 1.734723475976807094E-15 ) ) ;
#2536 = CARTESIAN_POINT ( 'NONE',  ( -11.18368045070454464, 76.64568724800108157, -7.561459486735044422 ) ) ;
#2537 = CARTESIAN_POINT ( 'NONE',  ( -11.67291695571009313, 80.18266643954832773, 6.796720356239053906 ) ) ;
#2538 = CARTESIAN_POINT ( 'NONE',  ( -7.409984580736203970E-16, 10.68000000000000149, 12.37355403259654985 ) ) ;
#2539 = DIRECTION ( 'NONE',  ( 0.000000000000000000, 0.000000000000000000, -1.000000000000000000 ) ) ;
#2540 = DIRECTION ( 'NONE',  ( 0.000000000000000000, 0.000000000000000000, 1.000000000000000000 ) ) ;
#2541 = CARTESIAN_POINT ( 'NONE',  ( -11.76794919243112325, 6.930000000000005933, -2.602085213965210642E-15 ) ) ;
#2542 = CARTESIAN_POINT ( 'NONE',  ( 2.272985001014427393E-15, 59.17999999999999261, -12.37355403259654807 ) ) ;
#2543 = CARTESIAN_POINT ( 'NONE',  ( -8.043339635997654113, -69.75624999999980957, 8.043339635996304082 ) ) ;
#2544 = CARTESIAN_POINT ( 'NONE',  ( -1.564113515457998572E-12, -29.13749999999993179, 18.62500000000000000 ) ) ;
#2545 = CARTESIAN_POINT ( 'NONE',  ( 13.50000000000000355, -11.42000000000000526, -4.386415899144233244 ) ) ;
#2546 = CARTESIAN_POINT ( 'NONE',  ( 2.138189944381238661, 34.75688142232025513, 13.50000000000000000 ) ) ;
#2547 = CARTESIAN_POINT ( 'NONE',  ( 8.363171565773356519, 75.86070654028085869, -10.59829022713068092 ) ) ;
#2548 = CARTESIAN_POINT ( 'NONE',  ( 10.92172942406179104, 68.73000000000000398, -7.935100905948385908 ) ) ;
#2549 = CARTESIAN_POINT ( 'NONE',  ( -7.272992578804310604, 36.37999999999998835, 10.01041549318726709 ) ) ;
#2550 = DIRECTION ( 'NONE',  ( -1.000000000000000000, 0.000000000000000000, -2.806191565803427284E-15 ) ) ;
#2551 = EDGE_CURVE ( 'NONE', #11530, #3044, #6962, .T. ) ;
#2552 = CARTESIAN_POINT ( 'NONE',  ( -10.83358975528349255, 58.62471529981993257, -8.055956318462602184 ) ) ;
#2553 = CARTESIAN_POINT ( 'NONE',  ( 2.445080149700053643E-15, 51.18000000000000682, -13.50000000000000000 ) ) ;
#2554 = CARTESIAN_POINT ( 'NONE',  ( 13.14266044583062332, 69.53951601861682263, -3.086384239676795538 ) ) ;
#2555 = CARTESIAN_POINT ( 'NONE',  ( -19.79695994079635213, 7.170708369609773314, 7.999999999999814371 ) ) ;
#2556 = CARTESIAN_POINT ( 'NONE',  ( 10.61848859199797168, 30.11238384093089948, 8.344967852243197370 ) ) ;
#2557 = CARTESIAN_POINT ( 'NONE',  ( -0.5765868356256266258, 55.20073193861872340, -13.48768407954960580 ) ) ;
#2558 = CARTESIAN_POINT ( 'NONE',  ( -4.997904479726364535, 50.49965712629579428, 12.54491501226717709 ) ) ;
#2559 = CARTESIAN_POINT ( 'NONE',  ( 13.36443380739206077, 63.49676886780871143, -1.908453827262113656 ) ) ;
#2560 = CARTESIAN_POINT ( 'NONE',  ( 8.019993042041946296, 42.87621988591261157, -10.85980660541363640 ) ) ;
#2561 = CARTESIAN_POINT ( 'NONE',  ( 10.63937102846270832, 39.11358967386987473, 8.313624546134036564 ) ) ;
#2562 = VERTEX_POINT ( 'NONE', #2260 ) ;
#2563 = CARTESIAN_POINT ( 'NONE',  ( -13.39749578736152102, 70.87207924715265506, -1.660457757727584527 ) ) ;
#2564 = CARTESIAN_POINT ( 'NONE',  ( -8.043339635996302306, -6.243749999999984368, -8.043339635997654113 ) ) ;
#2565 = VERTEX_POINT ( 'NONE', #15440 ) ;
#2566 = ORIENTED_EDGE ( 'NONE', *, *, #13461, .F. ) ;
#2567 = CARTESIAN_POINT ( 'NONE',  ( 8.343458848123583849, 18.88000000000000256, -11.48378591275253768 ) ) ;
#2568 = CARTESIAN_POINT ( 'NONE',  ( -7.714727599197335195, -88.45312499999978684, -18.62500000000064304 ) ) ;
#2569 = CARTESIAN_POINT ( 'NONE',  ( 4.672230816173793322, 61.01172198417896197, -12.66586740219305973 ) ) ;
#2570 = CARTESIAN_POINT ( 'NONE',  ( -13.49999999999999822, 15.07999999999999297, 4.386415899144235908 ) ) ;
#2571 = CARTESIAN_POINT ( 'NONE',  ( 4.228388219011975480, 71.83122618453306529, 12.85116208698753404 ) ) ;
#2572 = CARTESIAN_POINT ( 'NONE',  ( 13.37669266512173394, 57.36630447280914780, 1.821840660456907068 ) ) ;
#2573 = CARTESIAN_POINT ( 'NONE',  ( -7.272992578804310604, 72.38000000000000966, 10.01041549318726709 ) ) ;
#2574 = CARTESIAN_POINT ( 'NONE',  ( 7.272992578804308828, 72.98000000000000398, 10.01041549318726709 ) ) ;
#2575 = CARTESIAN_POINT ( 'NONE',  ( -3.779418409325009609, 47.54410635614043201, 12.96019630752388174 ) ) ;
#2576 = CARTESIAN_POINT ( 'NONE',  ( -4.171729424061791036, 46.53000000000000114, 12.83926296998457239 ) ) ;
#2577 = CARTESIAN_POINT ( 'NONE',  ( 12.56770389185380665, -100.0000000000000426, 12.75622125074128910 ) ) ;
#2578 = CARTESIAN_POINT ( 'NONE',  ( -4.448365178832009548, 10.00000000000000888, -12.11652676267665463 ) ) ;
#2579 = CARTESIAN_POINT ( 'NONE',  ( 11.37500000000000178, -92.64999999999974989, 9.531744055041752924E-13 ) ) ;
#2580 = CARTESIAN_POINT ( 'NONE',  ( 1.203083463835363736E-13, 37.18000000000000682, -13.50000000000000000 ) ) ;
#2581 = CARTESIAN_POINT ( 'NONE',  ( 13.07329398270627152, 33.54991537887530484, -3.368011412300191854 ) ) ;
#2582 = CARTESIAN_POINT ( 'NONE',  ( -1.904792500483675433, 73.24848043052601554, -13.36599649914418286 ) ) ;
#2583 = VERTEX_POINT ( 'NONE', #950 ) ;
#2584 = ORIENTED_EDGE ( 'NONE', *, *, #12599, .F. ) ;
#2585 = CARTESIAN_POINT ( 'NONE',  ( 11.76794919243112325, 79.28000000000000114, 3.823638476888997051 ) ) ;
#2586 = EDGE_LOOP ( 'NONE', ( #11460, #6153, #3710, #7044 ) ) ;
#2587 = VECTOR ( 'NONE', #6830, 1000.000000000000000 ) ;
#2588 = CARTESIAN_POINT ( 'NONE',  ( 8.043339635996298753, -105.0687499999997527, 8.043339635997652337 ) ) ;
#2589 = ADVANCED_FACE ( 'NONE', ( #4853 ), #14290, .T. ) ;
#2590 = CARTESIAN_POINT ( 'NONE',  ( -10.39000254332373530, 44.26011697933602562, 8.621106295591292934 ) ) ;
#2591 = CARTESIAN_POINT ( 'NONE',  ( 8.458421099448676372, 8.027996319639555622, 16.03410433562983428 ) ) ;
#2592 = CARTESIAN_POINT ( 'NONE',  ( -8.343458848123582072, 44.37999999999998835, 11.48378591275254124 ) ) ;
#2593 = CARTESIAN_POINT ( 'NONE',  ( -8.131449393936593495, 71.37121561422294747, 10.77635893735787853 ) ) ;
#2594 =( BOUNDED_CURVE ( )  B_SPLINE_CURVE ( 2, ( #15576, #14255, #5177, #17001, #3750, #10307, #7569, #14340, #9075, #2399, #13207, #8984, #17265 ),
 .UNSPECIFIED., .F., .F. ) 
 B_SPLINE_CURVE_WITH_KNOTS ( ( 3, 2, 2, 2, 2, 2, 3 ),
 ( 0.5801927019965731347, 0.5830229102989955559, 0.5886833269038401761, 0.5943437435086847964, 0.6000041601135294167, 0.6056645767183740370, 0.6084947812034886550 ),
 .UNSPECIFIED. ) 
 CURVE ( )  GEOMETRIC_REPRESENTATION_ITEM ( )  RATIONAL_B_SPLINE_CURVE ( ( 0.9755282581475767101, 0.9755282581475757109, 1.000000000000000000, 0.9510565162951535312, 1.000000000000000000, 0.9510565162951535312, 1.000000000000000000, 0.9510565162951535312, 1.000000000000000000, 0.9510565162951535312, 1.000000000000000000, 0.9755282911543938784, 0.9755282581476212300 ) ) 
 REPRESENTATION_ITEM ( '' )  );
#2595 = CARTESIAN_POINT ( 'NONE',  ( -7.714727599200466912, -20.84687499999993321, 18.62499999999935341 ) ) ;
#2596 = CARTESIAN_POINT ( 'NONE',  ( -13.09738736950409610, 67.81195449946297060, -3.320732649296348260 ) ) ;
#2597 = CARTESIAN_POINT ( 'NONE',  ( -13.16986379960055409, -3.156249999999973355, 13.16986379959834252 ) ) ;
#2598 = CARTESIAN_POINT ( 'NONE',  ( 12.68800670179988543, 54.59854656979176468, -4.665911999866591664 ) ) ;
#2599 = CARTESIAN_POINT ( 'NONE',  ( 11.76794919243112325, 17.28000000000001535, 3.823638476888996163 ) ) ;
#2600 = CARTESIAN_POINT ( 'NONE',  ( 13.16986379959834075, -97.81874999999976694, 13.16986379960055231 ) ) ;
#2601 = CARTESIAN_POINT ( 'NONE',  ( -13.49368735088633109, 64.91235305258140897, -0.5046298214861710818 ) ) ;
#2602 = CARTESIAN_POINT ( 'NONE',  ( -13.39406886664265350, 34.86875242566303967, -1.758890122878330242 ) ) ;
#2603 = VERTEX_POINT ( 'NONE', #17036 ) ;
#2604 = CYLINDRICAL_SURFACE ( 'NONE', #6183, 13.50000000000000000 ) ;
#2605 = CARTESIAN_POINT ( 'NONE',  ( -3.526462373425089947, 31.30679734055596342, -13.03315977265726389 ) ) ;
#2606 = DIRECTION ( 'NONE',  ( 0.000000000000000000, 0.000000000000000000, -1.000000000000000000 ) ) ;
#2607 = CARTESIAN_POINT ( 'NONE',  ( 11.76794919243112325, -9.720000000000005969, 3.823638476888996163 ) ) ;
#2608 = CARTESIAN_POINT ( 'NONE',  ( 3.543844789428542974, 59.80725957930280856, 13.02736174611344389 ) ) ;
#2609 = CARTESIAN_POINT ( 'NONE',  ( -13.49999999999999822, -9.220000000000002416, -4.386415899144240349 ) ) ;
#2610 = CARTESIAN_POINT ( 'NONE',  ( -1.158615910969277962, 53.63836784856319184, 13.45283109147737122 ) ) ;
#2611 = CARTESIAN_POINT ( 'NONE',  ( -9.520470885617717371, 51.22999999999999687, 6.917026985038133624 ) ) ;
#2612 = APPLICATION_PROTOCOL_DEFINITION ( 'draft international standard', 'automotive_design', 1998, #3256 ) ;
#2613 = CARTESIAN_POINT ( 'NONE',  ( -4.171729424061791036, 67.53000000000000114, 12.83926296998457239 ) ) ;
#2614 = CARTESIAN_POINT ( 'NONE',  ( 8.568141767261806763, 51.00872231198475504, 10.43334200729065131 ) ) ;
#2615 = PRODUCT_RELATED_PRODUCT_CATEGORY ( 'part', '', ( #6700 ) ) ;
#2616 = CARTESIAN_POINT ( 'NONE',  ( -12.93551790015123615, 37.79160025195344730, -3.863825158923987590 ) ) ;
#2617 = CARTESIAN_POINT ( 'NONE',  ( 13.30751972784499948, 36.35018164686414366, 2.271560209828621169 ) ) ;
#2618 = CARTESIAN_POINT ( 'NONE',  ( -18.62500000000000000, -32.22499999999993747, -1.562973063126292757E-12 ) ) ;
#2619 = CARTESIAN_POINT ( 'NONE',  ( -6.252194047236812935, 74.45099389143528867, 11.96513968989806642 ) ) ;
#2620 = CARTESIAN_POINT ( 'NONE',  ( -13.48669916444661254, 76.95072171427733565, 0.6016804198428439276 ) ) ;
#2621 = CARTESIAN_POINT ( 'NONE',  ( -13.04843550171840327, 80.05451087008829347, 3.490901052320607878 ) ) ;
#2622 = CARTESIAN_POINT ( 'NONE',  ( 7.272992578804311492, 11.88000000000000966, -10.01041549318726709 ) ) ;
#2623 = CARTESIAN_POINT ( 'NONE',  ( 7.500000000000000888, 104.2017679084708135, -9.199276322163095543 ) ) ;
#2624 = CARTESIAN_POINT ( 'NONE',  ( -4.171729424061791036, 8.530000000000010019, 12.83926296998457239 ) ) ;
#2625 = CARTESIAN_POINT ( 'NONE',  ( -11.76794919243112325, 6.779999999999995808, -3.823638476888998827 ) ) ;
#2626 = EDGE_CURVE ( 'NONE', #14369, #5101, #4644, .T. ) ;
#2627 = CARTESIAN_POINT ( 'NONE',  ( 7.272992578804311492, 49.88000000000000256, -10.01041549318726886 ) ) ;
#2628 = CARTESIAN_POINT ( 'NONE',  ( 11.37499999999960210, -32.25937499999992042, 4.711679271994918317 ) ) ;
#2629 = CARTESIAN_POINT ( 'NONE',  ( -18.62500000000064659, -42.66562499999989200, 7.714727599197335195 ) ) ;
#2630 = CARTESIAN_POINT ( 'NONE',  ( 8.343458848123583849, -8.119999999999999218, -11.48378591275253768 ) ) ;
#2631 = EDGE_CURVE ( 'NONE', #11029, #1687, #13403, .T. ) ;
#2632 = CARTESIAN_POINT ( 'NONE',  ( -10.28591867025567552, 40.59439376045062886, -8.743580910627192893 ) ) ;
#2633 = DIRECTION ( 'NONE',  ( 0.000000000000000000, 0.000000000000000000, 1.000000000000000000 ) ) ;
#2634 = CARTESIAN_POINT ( 'NONE',  ( 12.97379061124320643, 75.56364355911627229, -3.737309416985219901 ) ) ;
#2635 = CARTESIAN_POINT ( 'NONE',  ( -1.732050807569007977, 0.000000000000000000, 18.99999999999998224 ) ) ;
#2636 = CARTESIAN_POINT ( 'NONE',  ( -9.520470885617715595, 41.63000000000000256, -6.917026985038136289 ) ) ;
#2637 = CARTESIAN_POINT ( 'NONE',  ( -9.319118815187000138, 41.31534473877036362, 9.767498538115876983 ) ) ;
#2638 = CARTESIAN_POINT ( 'NONE',  ( -12.72549284276933612, 58.76724356285878059, -4.507839643634814486 ) ) ;
#2639 = DIRECTION ( 'NONE',  ( -0.000000000000000000, -1.000000000000000000, -0.000000000000000000 ) ) ;
#2640 = CARTESIAN_POINT ( 'NONE',  ( 0.000000000000000000, 80.93000000000000682, 0.000000000000000000 ) ) ;
#2641 = CARTESIAN_POINT ( 'NONE',  ( 1.108954987895778950E-11, 4.813974596216015200, 12.00000000000000178 ) ) ;
#2642 = CARTESIAN_POINT ( 'NONE',  ( -10.32427104660286510, 55.59635412314061398, -8.699356681262834456 ) ) ;
#2643 = CARTESIAN_POINT ( 'NONE',  ( -10.10486216940530646, 49.58475825896382361, -8.952216472663192093 ) ) ;
#2644 = CARTESIAN_POINT ( 'NONE',  ( 12.72780439611452685, 63.59248189055149680, -4.500512707593768980 ) ) ;
#2645 = B_SPLINE_CURVE_WITH_KNOTS ( 'NONE', 3,
 ( #6921, #7091, #9750, #14836 ),
 .UNSPECIFIED., .F., .F.,
 ( 4, 4 ),
 ( 2.376698214958262694E-07, 0.007646667280170311651 ),
 .UNSPECIFIED. ) ;
#2646 = CARTESIAN_POINT ( 'NONE',  ( 11.94735587504193397, 42.66220391500009868, -6.285819396456265196 ) ) ;
#2647 = CARTESIAN_POINT ( 'NONE',  ( 13.48226358575459471, 39.45385880521023125, -0.6919323233915973814 ) ) ;
#2648 = ORIENTED_EDGE ( 'NONE', *, *, #1385, .F. ) ;
#2649 = CARTESIAN_POINT ( 'NONE',  ( -13.39560391571467868, 70.87153809504057733, -1.675667837312355690 ) ) ;
#2650 = CARTESIAN_POINT ( 'NONE',  ( 0.000000000000000000, 5.918584287042170544, 0.000000000000000000 ) ) ;
#2651 = ORIENTED_EDGE ( 'NONE', *, *, #4834, .F. ) ;
#2652 = ADVANCED_FACE ( 'NONE', ( #5469 ), #7863, .T. ) ;
#2653 = VECTOR ( 'NONE', #3372, 1000.000000000000000 ) ;
#2654 = ORIENTED_EDGE ( 'NONE', *, *, #8764, .F. ) ;
#2655 = CARTESIAN_POINT ( 'NONE',  ( -4.171729424061787483, 22.33000000000001606, -12.83926296998457417 ) ) ;
#2656 = CARTESIAN_POINT ( 'NONE',  ( -18.62500000000064659, -75.96562499999980389, 7.714727599197335195 ) ) ;
#2657 = CARTESIAN_POINT ( 'NONE',  ( 11.56708140751954517, 60.68951295404890089, -6.960795543196039326 ) ) ;
#2658 = CARTESIAN_POINT ( 'NONE',  ( -8.343458848123582072, 9.379999999999999005, 11.48378591275254124 ) ) ;
#2659 = CARTESIAN_POINT ( 'NONE',  ( 7.631122679475396353, 71.96662365772242254, 11.13625026764144721 ) ) ;
#2660 = CARTESIAN_POINT ( 'NONE',  ( 13.35787352930365657, 57.49841857882535123, -1.953818782010021904 ) ) ;
#2661 = CARTESIAN_POINT ( 'NONE',  ( -7.272992578804310604, 66.37999999999999545, 10.01041549318726709 ) ) ;
#2662 = CARTESIAN_POINT ( 'NONE',  ( 11.76794919243112325, 76.42999999999999261, 1.441158131103945434E-15 ) ) ;
#2663 = CARTESIAN_POINT ( 'NONE',  ( -9.902832463360342174, 47.28584755916202909, 9.175181509501756594 ) ) ;
#2664 = CARTESIAN_POINT ( 'NONE',  ( -7.499999999999993783, -28.00000000000000000, -9.367496997597603681 ) ) ;
#2665 = CARTESIAN_POINT ( 'NONE',  ( 13.50000000000000355, 38.57999999999999829, -4.386415899144233244 ) ) ;
#2666 = FACE_OUTER_BOUND ( 'NONE', #17082, .T. ) ;
#2667 = CARTESIAN_POINT ( 'NONE',  ( 9.538709233711902776E-13, -80.16249999999979536, -11.37500000000000178 ) ) ;
#2668 = CARTESIAN_POINT ( 'NONE',  ( -10.92172942406178926, 51.62999999999999545, -7.935100905948389460 ) ) ;
#2669 = CARTESIAN_POINT ( 'NONE',  ( 10.37937675924905889, 33.76051463339396719, -8.632437102218030844 ) ) ;
#2670 = CARTESIAN_POINT ( 'NONE',  ( -6.569835995856939448, 73.42170974065275857, -11.80192330709520299 ) ) ;
#2671 = ORIENTED_EDGE ( 'NONE', *, *, #5983, .F. ) ;
#2672 = ORIENTED_EDGE ( 'NONE', *, *, #721, .T. ) ;
#2673 = B_SPLINE_CURVE_WITH_KNOTS ( 'NONE', 3,
 ( #6068, #3397, #11709, #7740, #3658, #14251, #2139, #9070, #16912, #4904, #11451, #7564, #17086, #3309, #8810, #4645, #11365, #15656, #8722, #5982, #8981, #14168, #10133, #2055, #14080, #14336, #14423, #4991, #1968, #7392, #10218, #2225, #10303, #6157, #15487, #11534, #15748, #4817, #12770, #659, #10393, #16825, #12941, #11623, #7479, #12860, #749, #2312, #15571, #3566, #7654, #13030, #3482, #8896, #16998, #824, #914, #6323, #10732, #4092, #12136, #14769, #16096, #5173, #25, #14852, #3835, #4004, #9421, #5263, #9507, #8004, #8176, #1340, #3918, #17432, #15925, #2660, #6590, #5428, #14509, #2396, #10565, #13370, #5345, #9249, #17261, #14602, #15840, #8090, #16180, #6757, #9161, #7831, #10649, #13454, #10818, #1179, #2482, #11970, #2746, #13203, #7915, #1003, #6414, #1089, #2572, #1259, #13290, #5086, #17351, #11798, #16012, #17175, #10480, #3746, #11887, #6504, #6671, #12054, #9335, #14684, #9859, #9945, #15031, #15206, #11171, #209, #7191, #15293, #16364, #5786, #16546, #293, #16634, #3012, #3195, #13881, #16457, #12494, #10996, #4538, #8354, #13540, #8533, #9594, #5614, #8442, #4452, #12225, #6847, #117, #15114, #1782, #5523, #1520, #10907, #11255, #1430, #16276, #13797, #1695, #7110, #4182, #4271, #14945, #2836, #2924, #8267, #13628, #3106, #6937, #12315, #9681, #13711, #1610, #12580, #5876, #7027, #12405, #5702, #11083, #4359, #468, #380 ),
 .UNSPECIFIED., .F., .F.,
 ( 4, 2, 2, 2, 1, 2, 2, 1, 2, 2, 2, 2, 1, 2, 2, 1, 1, 2, 2, 2, 2, 2, 2, 2, 2, 2, 2, 1, 1, 1, 1, 1, 1, 2, 2, 1, 2, 2, 2, 1, 2, 2, 1, 2, 2, 2, 2, 2, 1, 1, 2, 2, 2, 1, 2, 2, 1, 2, 1, 2, 2, 1, 1, 2, 2, 2, 2, 2, 1, 1, 1, 1, 1, 2, 2, 2, 2, 1, 1, 2, 2, 2, 2, 2, 2, 2, 2, 2, 2, 1, 2, 2, 1, 1, 1, 1, 2, 1, 2, 2, 1, 1, 2, 2, 2, 2, 1, 2, 2, 1, 1, 4 ),
 ( 0.4460935527485729302, 0.4470126776020930115, 0.4474722400288530522, 0.4477020212422330725, 0.4477594665455780776, 0.4477738278714143427, 0.4477881891972506079, 0.4478169118489230827, 0.4479318024556130928, 0.4488509273091330631, 0.4493104897358931038, 0.4494253803425830585, 0.4494541029942555888, 0.4494612836571736936, 0.4494684643200918539, 0.4494828256459280635, 0.4495402709492730686, 0.4497700521626530890, 0.4506891770161732258, 0.4516083018696933071, 0.4518380830830733275, 0.4520678642964533478, 0.4525274267232133885, 0.4534465515767335253, 0.4543656764302536066, 0.4544231217335986117, 0.4544805670369436168, 0.4545954576436336270, 0.4548252388570136473, 0.4552848012837737435, 0.4555145824971537638, 0.4556294731038437740, 0.4556869184071887791, 0.4557156410588613094, 0.4557300023846975190, 0.4557443637105337841, 0.4562039261372938248, 0.4566634885640538100, 0.4568932697774338303, 0.4569507150807788354, 0.4569650764066151005, 0.4569794377324513102, 0.4570081603841238405, 0.4571230509908138506, 0.4589613006978539023, 0.4594208631246138874, 0.4594495857762864177, 0.4594783084279588925, 0.4595357537313038976, 0.4596506443379939078, 0.4598804255513739281, 0.4603399879781339132, 0.4605697691915139336, 0.4606846597982039437, 0.4607133824498764740, 0.4607421051015489488, 0.4607995504048939539, 0.4617186752584139797, 0.4619484564717940001, 0.4619628177976302097, 0.4619771791234664748, 0.4620059017751390051, 0.4620633470784839547, 0.4621782376851739649, 0.4626378001119338945, 0.4635569249654538093, 0.4644760498189737241, 0.4644832304818918289, 0.4644904111448099893, 0.4645047724706462544, 0.4645334951223187292, 0.4645909404256636788, 0.4647058310323536889, 0.4649356122457336538, 0.4653951746724935834, 0.4663142995260133872, 0.4667738619527733168, 0.4668887525594632715, 0.4669461978628082766, 0.4669749205144807513, 0.4670036431661532816, 0.4672334243795331910, 0.4681525492330529392, 0.4690716740865726320, 0.4693014552999525413, 0.4695312365133325061, 0.4699907989400923247, 0.4709099237936120730, 0.4718290486471317657, 0.4719439392538217759, 0.4719726619054942507, 0.4719870232313305158, 0.4720013845571667255, 0.4720588298605117306, 0.4722886110738916954, 0.4727481735006515695, 0.4732077359274114992, 0.4732220972532477643, 0.4732292779161658691, 0.4732364585790839739, 0.4732651812307565042, 0.4733226265341014538, 0.4734375171407914640, 0.4736672983541714288, 0.4741268607809313584, 0.4743566419943113788, 0.4744715326010013334, 0.4744858939268375986, 0.4745002552526738082, 0.4745289779043463385, 0.4745864232076913436, 0.4755055480612112584 ),
 .UNSPECIFIED. ) ;
#2674 = VERTEX_POINT ( 'NONE', #16046 ) ;
#2675 = EDGE_CURVE ( 'NONE', #4872, #4556, #17316, .T. ) ;
#2676 = CARTESIAN_POINT ( 'NONE',  ( 8.043339635997652337, -75.93124999999983515, -8.043339635996302306 ) ) ;
#2677 = CARTESIAN_POINT ( 'NONE',  ( -0.3134612214510462680, 44.66872117570036949, 13.49736608497514645 ) ) ;
#2678 = CARTESIAN_POINT ( 'NONE',  ( -7.499999999999995559, -27.69291120311264720, 2.544524385544278289 ) ) ;
#2679 = CARTESIAN_POINT ( 'NONE',  ( 8.343458848123578520, 38.97999999999998266, 11.48378591275254124 ) ) ;
#2680 = CARTESIAN_POINT ( 'NONE',  ( -13.50006591323950289, 70.92792592063743484, -0.06117401498312825814 ) ) ;
#2681 = CIRCLE ( 'NONE', #4967, 26.00000000000000355 ) ;
#2682 = B_SPLINE_CURVE_WITH_KNOTS ( 'NONE', 3,
 ( #14801, #8214, #12001, #2693, #13660, #1554, #3953, #9366, #14716, #13402, #16127, #4038, #13490, #14890, #1378, #9452, #6793, #12173, #8304, #16217, #13576, #64, #5467, #11031, #9630, #12259, #154, #5560 ),
 .UNSPECIFIED., .F., .F.,
 ( 4, 2, 2, 2, 2, 2, 2, 2, 2, 2, 2, 2, 2, 4 ),
 ( 0.003365197809828101606, 0.004806483441736369121, 0.006247769073644636635, 0.007689054705552904150, 0.009130340337461170797, 0.01201291160127770236, 0.01489548286509423738, 0.01633676849700250316, 0.01777805412891076894, 0.01921933976081903125, 0.02066062539272729703, 0.02354319665654382859, 0.02498448228845209437, 0.02642576792036036015 ),
 .UNSPECIFIED. ) ;
#2683 = CARTESIAN_POINT ( 'NONE',  ( -7.714727599197334307, -31.25312499999991545, -18.62500000000064659 ) ) ;
#2684 = CARTESIAN_POINT ( 'NONE',  ( -11.67270096012221714, 68.18223154335983338, 6.782186488376318323 ) ) ;
#2685 = CARTESIAN_POINT ( 'NONE',  ( -7.714727599200466912, -4.196874999999971934, 18.62499999999935341 ) ) ;
#2686 = CARTESIAN_POINT ( 'NONE',  ( 13.06145935877203001, 54.55171067861751055, -3.416583277388366202 ) ) ;
#2687 = CARTESIAN_POINT ( 'NONE',  ( -9.520470885617715595, 15.63000000000000433, -6.917026985038136289 ) ) ;
#2688 = CARTESIAN_POINT ( 'NONE',  ( -2.811464633627016061E-07, 74.67999216907730897, 13.49999999999999289 ) ) ;
#2689 = CARTESIAN_POINT ( 'NONE',  ( -13.38153342487016673, 64.99234170124786658, 1.784551494147652795 ) ) ;
#2690 = CARTESIAN_POINT ( 'NONE',  ( -12.91999168696053779, 34.78966554277187129, -3.915358232556644946 ) ) ;
#2691 = CARTESIAN_POINT ( 'NONE',  ( 8.343458848123578520, 21.98000000000001108, 11.48378591275254124 ) ) ;
#2692 = ORIENTED_EDGE ( 'NONE', *, *, #482, .F. ) ;
#2693 = CARTESIAN_POINT ( 'NONE',  ( -0.7905400041755126228, 1.593905776373958320E-15, -12.11837741667673285 ) ) ;
#2694 = MECHANICAL_DESIGN_GEOMETRIC_PRESENTATION_REPRESENTATION (  '', ( #12602 ), #12880 ) ;
#2695 = CARTESIAN_POINT ( 'NONE',  ( -5.815297001295619772, 31.39166481203774239, -12.18434089980365442 ) ) ;
#2696 = CARTESIAN_POINT ( 'NONE',  ( 6.123937747468421122, 72.95612668926172262, -12.03133095083381221 ) ) ;
#2697 = CARTESIAN_POINT ( 'NONE',  ( 3.636496289402154414, -13.17000000000000171, 11.19198476289190758 ) ) ;
#2698 = CARTESIAN_POINT ( 'NONE',  ( 23.28534784291398552, 6.548267719634617734, 4.206197538246546408 ) ) ;
#2699 = CARTESIAN_POINT ( 'NONE',  ( -13.49999999999999822, -14.92000000000000171, 4.386415899144235908 ) ) ;
#2700 =( BOUNDED_CURVE ( )  B_SPLINE_CURVE ( 2, ( #10226, #5836, #14260, #11219, #8580, #1825, #2149, #7573, #12951, #834, #6245, #14993, #17269 ),
 .UNSPECIFIED., .F., .F. ) 
 B_SPLINE_CURVE_WITH_KNOTS ( ( 3, 2, 2, 2, 2, 2, 3 ),
 ( 0.09722222222222222376, 0.1000000000000000056, 0.1055555555555555552, 0.1111111111111111049, 0.1166666666666666685, 0.1222222222222222182, 0.1249999999999999861 ),
 .UNSPECIFIED. ) 
 CURVE ( )  GEOMETRIC_REPRESENTATION_ITEM ( )  RATIONAL_B_SPLINE_CURVE ( ( 0.9755282581475768211, 0.9755282581475768211, 1.000000000000000000, 0.9510565162951535312, 1.000000000000000000, 0.9510565162951535312, 1.000000000000000000, 0.9510565162951535312, 1.000000000000000000, 0.9510565162951535312, 1.000000000000000000, 0.9755282581475768211, 0.9755282581475768211 ) ) 
 REPRESENTATION_ITEM ( '' )  );
#2701 = CARTESIAN_POINT ( 'NONE',  ( -13.45991843043591096, 52.96599441791912000, 1.039553241502096492 ) ) ;
#2702 = CARTESIAN_POINT ( 'NONE',  ( 11.76794919243112325, 49.42999999999999972, 1.441158131103945434E-15 ) ) ;
#2703 = CARTESIAN_POINT ( 'NONE',  ( 4.171729424061789260, 67.82999999999999829, 12.83926296998457417 ) ) ;
#2704 = CARTESIAN_POINT ( 'NONE',  ( 8.159022896083504506, 50.99002612469284657, 10.75553822827256667 ) ) ;
#2705 = VECTOR ( 'NONE', #5945, 1000.000000000000000 ) ;
#2706 = CARTESIAN_POINT ( 'NONE',  ( -8.560159368989697981, 37.50835171243769395, -10.44038914743977919 ) ) ;
#2707 = CARTESIAN_POINT ( 'NONE',  ( 13.48543408635378960, 36.40015360244564846, 0.8552198172808073151 ) ) ;
#2708 = CARTESIAN_POINT ( 'NONE',  ( 11.37499999999999645, -107.1499999999997783, 9.531744055041752924E-13 ) ) ;
#2709 = CARTESIAN_POINT ( 'NONE',  ( -12.98187037175444480, 74.06246690446607772, 3.705372543562173604 ) ) ;
#2710 = CARTESIAN_POINT ( 'NONE',  ( -11.15111956154761153, 76.64367872175508012, -7.609542610069594204 ) ) ;
#2711 = CARTESIAN_POINT ( 'NONE',  ( -13.50011421399957534, 79.90048673417217628, -0.8580047538210755498 ) ) ;
#2712 = CARTESIAN_POINT ( 'NONE',  ( 2.279995255611139653E-15, 12.17999999999999972, -12.37355403259654985 ) ) ;
#2713 = CARTESIAN_POINT ( 'NONE',  ( -6.556136581996924839, 80.92999999999997840, 10.79013235404389803 ) ) ;
#2714 = LINE ( 'NONE', #5489, #6668 ) ;
#2715 = CARTESIAN_POINT ( 'NONE',  ( 3.636496289402154414, -1.170000000000004370, 11.19198476289190758 ) ) ;
#2716 = CARTESIAN_POINT ( 'NONE',  ( -3.636496289402153081, 50.32999999999999829, -11.19198476289190936 ) ) ;
#2717 = CARTESIAN_POINT ( 'NONE',  ( -4.711679271994916540, -61.39687499999984510, 11.37499999999960210 ) ) ;
#2718 = FACE_OUTER_BOUND ( 'NONE', #17231, .T. ) ;
#2719 = CARTESIAN_POINT ( 'NONE',  ( -4.171729424061791036, -12.46999999999999531, 12.83926296998457239 ) ) ;
#2720 = CARTESIAN_POINT ( 'NONE',  ( -12.16229058013323971, 40.71428809225115941, -5.874955487704208501 ) ) ;
#2721 = DIRECTION ( 'NONE',  ( 0.000000000000000000, 0.000000000000000000, 1.000000000000000000 ) ) ;
#2722 = CARTESIAN_POINT ( 'NONE',  ( 11.36553548705029115, 75.15715277410380679, 7.285283613151663396 ) ) ;
#2723 = FACE_OUTER_BOUND ( 'NONE', #6773, .T. ) ;
#2724 = CARTESIAN_POINT ( 'NONE',  ( -9.520470885617715595, 44.62999999999999545, -6.917026985038136289 ) ) ;
#2725 = CARTESIAN_POINT ( 'NONE',  ( -11.25855217171127798, 41.20965883259114548, 7.449731759125929109 ) ) ;
#2726 = CARTESIAN_POINT ( 'NONE',  ( -5.791125120803746640, 58.39073047950922302, -12.19479843928588281 ) ) ;
#2727 = EDGE_CURVE ( 'NONE', #13554, #8820, #5229, .T. ) ;
#2728 = CARTESIAN_POINT ( 'NONE',  ( -9.708203932499369415, 9.496025403784438268, -7.053423027509682086 ) ) ;
#2729 = CARTESIAN_POINT ( 'NONE',  ( 4.171729424061791924, 60.03000000000000114, -12.83926296998457239 ) ) ;
#2730 = CYLINDRICAL_SURFACE ( 'NONE', #13801, 9.000000000000000000 ) ;
#2731 = CARTESIAN_POINT ( 'NONE',  ( -0.2755667434418575534, 55.18990795935741289, -13.49760167474381589 ) ) ;
#2732 = CARTESIAN_POINT ( 'NONE',  ( -12.38440713219831935, 49.73388119143891117, -5.378281758800909529 ) ) ;
#2733 = CARTESIAN_POINT ( 'NONE',  ( 11.58332279299003709, 63.68852283645756529, -6.934441872440040733 ) ) ;
#2734 = CARTESIAN_POINT ( 'NONE',  ( 10.70653119882778093, 42.11765279685179308, 8.223170724734634618 ) ) ;
#2735 = CARTESIAN_POINT ( 'NONE',  ( 5.972384284050402670, 38.89754117051403881, 12.11500310741538478 ) ) ;
#2736 = ORIENTED_EDGE ( 'NONE', *, *, #9055, .T. ) ;
#2737 = CARTESIAN_POINT ( 'NONE',  ( 8.343458848123583849, 74.87999999999999545, -11.48378591275253768 ) ) ;
#2738 = CARTESIAN_POINT ( 'NONE',  ( -4.171729424061787483, 48.32999999999999829, -12.83926296998457417 ) ) ;
#2739 = CARTESIAN_POINT ( 'NONE',  ( 13.50000000000000355, 15.57999999999999119, -4.386415899144233244 ) ) ;
#2740 = VERTEX_POINT ( 'NONE', #14652 ) ;
#2741 = CARTESIAN_POINT ( 'NONE',  ( -5.678969180980832476, 43.38635333003058037, -12.24742126128782793 ) ) ;
#2742 = CARTESIAN_POINT ( 'NONE',  ( 5.896062637422001984, 80.92999999999999261, -12.11648925032761070 ) ) ;
#2743 = CARTESIAN_POINT ( 'NONE',  ( 6.457115167747857321, 60.94273233830644898, -11.85567478446476208 ) ) ;
#2744 = CARTESIAN_POINT ( 'NONE',  ( -10.92172942406178926, 11.63000000000000078, -7.935100905948389460 ) ) ;
#2745 = FACE_OUTER_BOUND ( 'NONE', #4037, .T. ) ;
#2746 = CARTESIAN_POINT ( 'NONE',  ( 13.39657427826484692, 57.37181503160490337, 1.667884572635154772 ) ) ;
#2747 = CARTESIAN_POINT ( 'NONE',  ( 2.272985001014427788E-15, 68.18000000000000682, -12.37355403259654985 ) ) ;
#2748 = CARTESIAN_POINT ( 'NONE',  ( -3.636496289402153081, 77.32999999999999829, -11.19198476289190936 ) ) ;
#2749 = CARTESIAN_POINT ( 'NONE',  ( -9.452515638101248285, 47.30908623721830253, 9.648130606565771927 ) ) ;
#2750 = PLANE ( 'NONE',  #7593 ) ;
#2751 = CARTESIAN_POINT ( 'NONE',  ( -17.42428528562830436, 0.000000000000000000, -19.29752010712870813 ) ) ;
#2752 = ADVANCED_FACE ( 'NONE', ( #6814 ), #12021, .F. ) ;
#2753 = CIRCLE ( 'NONE', #7303, 4.000000000000000000 ) ;
#2754 = CARTESIAN_POINT ( 'NONE',  ( -11.88920123096388792, 9.999999999999994671, -1.626927807140451154 ) ) ;
#2755 = CARTESIAN_POINT ( 'NONE',  ( -4.711679271993004292, -71.80312499999982379, -11.37500000000039435 ) ) ;
#2756 = CARTESIAN_POINT ( 'NONE',  ( 0.000000000000000000, 0.000000000000000000, 0.000000000000000000 ) ) ;
#2757 = CARTESIAN_POINT ( 'NONE',  ( 13.08972554372986075, 33.54752892044167822, -3.303546669638452116 ) ) ;
#2758 = CARTESIAN_POINT ( 'NONE',  ( -9.668918040932872771, 73.56214475094522243, -9.421380043680995797 ) ) ;
#2759 = CARTESIAN_POINT ( 'NONE',  ( -8.000000000000145661, 0.000000000000000000, 17.32050807568870709 ) ) ;
#2760 = ORIENTED_EDGE ( 'NONE', *, *, #3222, .T. ) ;
#2761 = CARTESIAN_POINT ( 'NONE',  ( -1.878130797603207114, 62.61247834605533313, 13.36956684767648973 ) ) ;
#2762 = ORIENTED_EDGE ( 'NONE', *, *, #8980, .T. ) ;
#2763 = CARTESIAN_POINT ( 'NONE',  ( -11.37500000000039613, -99.86562499999978115, 4.711679271993000739 ) ) ;
#2764 = CARTESIAN_POINT ( 'NONE',  ( -12.00637140143189541, 44.15767552562060416, 6.172567600639201402 ) ) ;
#2765 = CARTESIAN_POINT ( 'NONE',  ( 10.99999999999990941, 7.773118517290098062, 15.58845726811995824 ) ) ;
#2766 = AXIS2_PLACEMENT_3D ( 'NONE', #14543, #8930, #10426 ) ;
#2767 = CARTESIAN_POINT ( 'NONE',  ( -10.92172942406179104, 47.23000000000000398, 7.935100905948387684 ) ) ;
#2768 = CARTESIAN_POINT ( 'NONE',  ( 4.171729424061789260, 43.82999999999999829, 12.83926296998457417 ) ) ;
#2769 = CARTESIAN_POINT ( 'NONE',  ( -13.21610071135663311, 71.02858066329746123, 2.789574207621230872 ) ) ;
#2770 = EDGE_CURVE ( 'NONE', #860, #14305, #14259, .T. ) ;
#2771 = AXIS2_PLACEMENT_3D ( 'NONE', #589, #12876, #5999 ) ;
#2772 = CARTESIAN_POINT ( 'NONE',  ( -18.62500000000064659, -52.06562499999986926, 7.714727599197333419 ) ) ;
#2773 = CARTESIAN_POINT ( 'NONE',  ( -13.20639446093759695, 67.82980414093228205, -2.833402894642628400 ) ) ;
#2774 = CARTESIAN_POINT ( 'NONE',  ( 13.16986379960055409, -28.13124999999991260, -13.16986379959834430 ) ) ;
#2775 = CARTESIAN_POINT ( 'NONE',  ( 11.52508508714884705, 54.69232931852840807, -7.030130978255333396 ) ) ;
#2776 = CIRCLE ( 'NONE', #17458, 26.00000000000000355 ) ;
#2777 = FACE_OUTER_BOUND ( 'NONE', #14696, .T. ) ;
#2778 = CARTESIAN_POINT ( 'NONE',  ( -11.86422739765571599, 64.69155293540576679, -6.441358199379890515 ) ) ;
#2779 = ORIENTED_EDGE ( 'NONE', *, *, #75, .T. ) ;
#2780 = CARTESIAN_POINT ( 'NONE',  ( -10.92172942406178926, 63.63000000000000256, -7.935100905948389460 ) ) ;
#2781 = CARTESIAN_POINT ( 'NONE',  ( -13.50004905279464751, 34.92235202864698351, -0.2160710017874167832 ) ) ;
#2782 = ORIENTED_EDGE ( 'NONE', *, *, #7001, .F. ) ;
#2783 = CARTESIAN_POINT ( 'NONE',  ( 13.40346092485427576, 78.37380768283490795, 1.611608511483868966 ) ) ;
#2784 = CARTESIAN_POINT ( 'NONE',  ( -8.891200544363830713E-16, 49.67999999999999261, 13.50000000000000000 ) ) ;
#2785 = CARTESIAN_POINT ( 'NONE',  ( 7.500000000000001776, -22.51612366527185927, 9.346045933502388436 ) ) ;
#2786 = CARTESIAN_POINT ( 'NONE',  ( 8.443682917512239428, 72.85701949107047426, -10.53438822433166422 ) ) ;
#2787 = CARTESIAN_POINT ( 'NONE',  ( 7.272992578804308828, -10.02000000000000490, 10.01041549318726709 ) ) ;
#2788 = CARTESIAN_POINT ( 'NONE',  ( 5.983891046846114392, 59.89805057951193135, 12.10717649698468001 ) ) ;
#2789 = CARTESIAN_POINT ( 'NONE',  ( -13.49999999999999822, -12.22000000000000774, -4.386415899144240349 ) ) ;
#2790 = CARTESIAN_POINT ( 'NONE',  ( -4.171729424061791036, 74.53000000000000114, 12.83926296998457239 ) ) ;
#2791 = CARTESIAN_POINT ( 'NONE',  ( -13.43529243779076765, 52.88326165438618887, -1.348469057933256110 ) ) ;
#2792 = VECTOR ( 'NONE', #14285, 1000.000000000000114 ) ;
#2793 = CARTESIAN_POINT ( 'NONE',  ( 2.272985001014427788E-15, 50.17999999999999261, -12.37355403259654985 ) ) ;
#2794 = CARTESIAN_POINT ( 'NONE',  ( -4.171729424061791036, 70.53000000000001535, 12.83926296998457239 ) ) ;
#2795 = CARTESIAN_POINT ( 'NONE',  ( 8.299058230608185482, 50.99636966829371687, 10.64802582075173021 ) ) ;
#2796 = CARTESIAN_POINT ( 'NONE',  ( -11.99645458172713752, 37.70142398792544469, -6.195780018836668290 ) ) ;
#2797 = CARTESIAN_POINT ( 'NONE',  ( 13.15610773373603948, 36.32156525380936074, 3.060187894280851140 ) ) ;
#2798 = CARTESIAN_POINT ( 'NONE',  ( -4.711679271994915652, -85.29687499999980105, 11.37499999999960210 ) ) ;
#2799 = CARTESIAN_POINT ( 'NONE',  ( -10.47229713462876610, 74.25542378161327406, 8.519458686554706617 ) ) ;
#2800 = CARTESIAN_POINT ( 'NONE',  ( -13.22110634326003975, 76.83180770776795043, -2.777616017796241898 ) ) ;
#2801 = CARTESIAN_POINT ( 'NONE',  ( -12.31517163679457916, 80.13229876729300827, 5.530790380342764045 ) ) ;
#2802 = CARTESIAN_POINT ( 'NONE',  ( -7.779800476318354832E-16, 7.813974596215564006, 12.00000000000000355 ) ) ;
#2803 = CARTESIAN_POINT ( 'NONE',  ( 0.000000000000000000, 80.93000000000000682, 0.000000000000000000 ) ) ;
#2804 = CARTESIAN_POINT ( 'NONE',  ( -3.636496289402156190, -1.469999999999999085, 11.19198476289190758 ) ) ;
#2805 = CARTESIAN_POINT ( 'NONE',  ( 2.272985001014427393E-15, 44.17999999999999261, -12.37355403259654807 ) ) ;
#2806 = CARTESIAN_POINT ( 'NONE',  ( 18.62500000000000000, -16.64999999999995950, 1.560692158462880521E-12 ) ) ;
#2807 =( BOUNDED_CURVE ( )  B_SPLINE_CURVE ( 2, ( #15726, #10285, #9140, #7631, #980, #3634, #14488 ),
 .UNSPECIFIED., .F., .F. ) 
 B_SPLINE_CURVE_WITH_KNOTS ( ( 3, 2, 2, 3 ),
 ( 2.168404344971008868E-19, 0.005875474857718830310, 0.01338919962976012172, 0.01714606201576732852 ),
 .UNSPECIFIED. ) 
 CURVE ( )  GEOMETRIC_REPRESENTATION_ITEM ( )  RATIONAL_B_SPLINE_CURVE ( ( 0.9833107263962475031, 0.9617278757631589903, 1.000000000000000000, 0.9510565162951535312, 1.000000000000000000, 0.9755282581476645287, 0.9755282581475768211 ) ) 
 REPRESENTATION_ITEM ( '' )  );
#2808 = CARTESIAN_POINT ( 'NONE',  ( -8.549982208541774191E-16, -12.32000000000000384, 14.19474002721660355 ) ) ;
#2809 = CARTESIAN_POINT ( 'NONE',  ( -2.380112485275091228, 34.26557354401293765, -13.29211986648399524 ) ) ;
#2810 = CARTESIAN_POINT ( 'NONE',  ( 13.32771338909670611, 75.35456652835816271, 2.149902385128953597 ) ) ;
#2811 = EDGE_CURVE ( 'NONE', #6836, #1275, #6454, .T. ) ;
#2812 = CARTESIAN_POINT ( 'NONE',  ( 3.119116752841613938, 2.511656448626852424E-16, -14.83158588741119388 ) ) ;
#2813 = CARTESIAN_POINT ( 'NONE',  ( -7.499999999999992895, 88.93000000000000682, -9.367496997597603681 ) ) ;
#2814 = CARTESIAN_POINT ( 'NONE',  ( -4.151018824075187297, 41.53077687151799324, 12.84636745817926773 ) ) ;
#2815 = VECTOR ( 'NONE', #4710, 1000.000000000000000 ) ;
#2816 = CARTESIAN_POINT ( 'NONE',  ( -5.763218716402632502, 58.38963670260850591, -12.20800189707574113 ) ) ;
#2817 = CARTESIAN_POINT ( 'NONE',  ( 0.000000000000000000, 0.000000000000000000, -22.50000000000000355 ) ) ;
#2818 = CARTESIAN_POINT ( 'NONE',  ( 0.000000000000000000, 9.999999999999998224, -14.50000000000000000 ) ) ;
#2819 = PLANE ( 'NONE',  #11564 ) ;
#2820 = CARTESIAN_POINT ( 'NONE',  ( -8.343458848123582072, 58.38000000000000966, 11.48378591275253768 ) ) ;
#2821 = CARTESIAN_POINT ( 'NONE',  ( -13.47670514672201492, 49.90263017273650092, -0.7938299215749298199 ) ) ;
#2822 = CARTESIAN_POINT ( 'NONE',  ( 13.40301953286001257, 63.37151237674334681, 1.680986317143484232 ) ) ;
#2823 = CARTESIAN_POINT ( 'NONE',  ( 11.28856919156083904, 42.15232267161604796, 7.408146303404825161 ) ) ;
#2824 = CARTESIAN_POINT ( 'NONE',  ( 1.785599194582236620E-06, 38.68004968046676595, 13.49999999999976374 ) ) ;
#2825 = ORIENTED_EDGE ( 'NONE', *, *, #2906, .F. ) ;
#2826 = CARTESIAN_POINT ( 'NONE',  ( -9.708203932499369415, 3.496025403784432051, -7.053423027509682086 ) ) ;
#2827 = CARTESIAN_POINT ( 'NONE',  ( -19.29752010712864418, 0.000000000000000000, 17.42428528562836831 ) ) ;
#2828 = CARTESIAN_POINT ( 'NONE',  ( -13.49999999999999822, 11.08000000000000540, 4.386415899144235908 ) ) ;
#2829 = ORIENTED_EDGE ( 'NONE', *, *, #12929, .T. ) ;
#2830 = CARTESIAN_POINT ( 'NONE',  ( -3.553968802922996773, 43.30778666167008595, -13.03033527728538310 ) ) ;
#2831 = CARTESIAN_POINT ( 'NONE',  ( -7.499999999999998224, 108.1058439696177516, 5.080312676971231234 ) ) ;
#2832 = CARTESIAN_POINT ( 'NONE',  ( 13.01319014679174479, 60.55827135456127053, -3.592833797878408841 ) ) ;
#2833 = CARTESIAN_POINT ( 'NONE',  ( 4.171729424061789260, 12.83000000000000895, 12.83926296998457239 ) ) ;
#2834 = CARTESIAN_POINT ( 'NONE',  ( -7.714727599197334307, -21.85312499999994884, -18.62500000000064304 ) ) ;
#2835 = CARTESIAN_POINT ( 'NONE',  ( 13.41802420445356425, 66.48176821741365927, -1.487227729902038220 ) ) ;
#2836 = CARTESIAN_POINT ( 'NONE',  ( 3.222688025018089597, 56.79589291944066787, 13.10971560064693620 ) ) ;
#2837 = CARTESIAN_POINT ( 'NONE',  ( -11.76794919243112325, 59.77999999999998693, -3.823638476888998827 ) ) ;
#2838 = CARTESIAN_POINT ( 'NONE',  ( -3.636496289402153081, 65.32999999999999829, -11.19198476289190936 ) ) ;
#2839 = CARTESIAN_POINT ( 'NONE',  ( -11.28838743354254959, 47.20770152966969846, 7.404409973131605760 ) ) ;
#2840 = CARTESIAN_POINT ( 'NONE',  ( 5.558388671817832360, 45.97832039020661199, -12.30261423939740162 ) ) ;
#2841 = DIRECTION ( 'NONE',  ( 0.000000000000000000, 0.000000000000000000, -1.000000000000000000 ) ) ;
#2842 = CARTESIAN_POINT ( 'NONE',  ( 3.856686604160783904, -100.0000000000000426, 13.67982212280359455 ) ) ;
#2843 = CARTESIAN_POINT ( 'NONE',  ( -3.677005786994592906, 56.54778140968930700, 12.98976059619792522 ) ) ;
#2844 = CARTESIAN_POINT ( 'NONE',  ( -4.711679271994916540, -94.69687499999979252, 11.37499999999960210 ) ) ;
#2845 = CARTESIAN_POINT ( 'NONE',  ( -2.138189944381236884, 39.25688142232026223, -13.50000000000000000 ) ) ;
#2846 = CARTESIAN_POINT ( 'NONE',  ( 10.42437936642323137, 33.75805611468842926, -8.578056805215203084 ) ) ;
#2847 = DIRECTION ( 'NONE',  ( -0.000000000000000000, 1.000000000000000000, -0.000000000000000000 ) ) ;
#2848 = CARTESIAN_POINT ( 'NONE',  ( 19.00000000000000711, 0.000000000000000000, -1.732050807568807027 ) ) ;
#2849 = ORIENTED_EDGE ( 'NONE', *, *, #11426, .F. ) ;
#2850 = CARTESIAN_POINT ( 'NONE',  ( -0.6030540269933777342, 62.65833043166017546, 13.50000000000103562 ) ) ;
#2851 = ORIENTED_EDGE ( 'NONE', *, *, #2727, .T. ) ;
#2852 = CARTESIAN_POINT ( 'NONE',  ( -13.47581441816511116, 40.90212384545007751, -0.8079750235031136762 ) ) ;
#2853 = CARTESIAN_POINT ( 'NONE',  ( 18.62499999999935341, -56.15937499999989058, 7.714727599200469577 ) ) ;
#2854 = CARTESIAN_POINT ( 'NONE',  ( -13.47719069686192839, 43.95707978810331440, 0.7844768294817338061 ) ) ;
#2855 = EDGE_CURVE ( 'NONE', #5187, #7222, #2714, .T. ) ;
#2856 = VECTOR ( 'NONE', #4357, 1000.000000000000000 ) ;
#2857 = CARTESIAN_POINT ( 'NONE',  ( 10.92172942406178926, 0.1300000000000051115, 7.935100905948385908 ) ) ;
#2858 = CARTESIAN_POINT ( 'NONE',  ( -13.50000000000000000, 40.92999999999999261, -3.306546357697853733E-15 ) ) ;
#2859 = CARTESIAN_POINT ( 'NONE',  ( -4.171729424061787483, 45.33000000000000540, -12.83926296998457417 ) ) ;
#2860 = CARTESIAN_POINT ( 'NONE',  ( -12.67307004936112413, 71.09835393786092084, 4.654973291148522208 ) ) ;
#2861 = CARTESIAN_POINT ( 'NONE',  ( -13.16986379959834252, -32.29374999999990337, -13.16986379960055409 ) ) ;
#2862 = CARTESIAN_POINT ( 'NONE',  ( -9.811400904590312777, 67.56937204541171127, -9.274875428382246767 ) ) ;
#2863 = CARTESIAN_POINT ( 'NONE',  ( -7.714727599197334307, -47.90312499999986784, -18.62500000000064659 ) ) ;
#2864 = AXIS2_PLACEMENT_3D ( 'NONE', #3359, #14215, #11238 ) ;
#2865 = CARTESIAN_POINT ( 'NONE',  ( 13.49994682080826713, 54.43208894843145629, -0.06111802256781772441 ) ) ;
#2866 = B_SPLINE_CURVE_WITH_KNOTS ( 'NONE', 3,
 ( #17179, #6508, #10483, #10568, #2144, #15844, #11890, #3838, #9252, #2485, #7919, #17435, #10999, #13458, #4009, #14949, #12058, #5348, #2575, #9510, #6674, #16015, #16183, #13373, #120, #13543, #12139, #5526, #17354, #14688, #10735, #4095, #12319, #16099, #9424, #5267, #16367, #9338, #28, #1433, #5432, #14773, #212, #1523, #2749, #5617, #6760, #6593, #1182, #8094, #10910, #2663, #4185, #8007, #10821, #14855, #1345, #15035, #8181, #2839, #6851, #12228, #16279, #11973, #10652, #9597, #3921, #1263, #8357, #8271, #13631, #6940, #4275, #2927, #9685, #296, #16721, #12408, #4628, #15469, #7374, #471, #3109, #5790, #1785, #6052, #12583, #7030, #5705, #1949, #3016, #13715, #8447, #13800, #16460, #16637, #1614, #7283, #11434, #3379, #11175, #4362, #15383, #9948, #5880, #11088, #9772, #12752, #1699, #15117, #7113, #12499, #385, #4543, #16549, #12666, #16806, #4455, #9862, #555, #15211, #15297, #8536, #13973, #13886, #7196, #11259, #3199, #4713, #8619, #1868, #5965, #11346, #10035, #641, #3290, #8705, #14065, #10116, #8815, #1971, #316, #13907, #7304, #10139, #1802, #1633, #14085, #15141, #11196, #8641, #16741, #5725, #12430, #11107, #3219, #7396, #16480, #7133, #4384, #16831, #9968, #12521, #3038, #9883, #13819, #12776, #8469, #4649, #13994, #15233, #9794, #1720, #10055, #4735, #3402, #4562, #4477, #405, #15407, #11455, #1889, #492, #5812, #8554, #15316, #6075, #12688, #577, #16571, #5898, #5987 ),
 .UNSPECIFIED., .F., .F.,
 ( 4, 2, 2, 1, 1, 2, 2, 2, 2, 2, 1, 2, 2, 1, 2, 2, 2, 2, 1, 1, 2, 2, 1, 2, 2, 2, 2, 2, 2, 2, 1, 1, 1, 2, 2, 2, 2, 1, 1, 1, 2, 2, 2, 2, 2, 2, 2, 2, 2, 1, 2, 2, 1, 1, 1, 2, 2, 2, 2, 2, 1, 2, 2, 2, 2, 2, 1, 1, 1, 2, 2, 2, 2, 1, 1, 2, 2, 1, 1, 2, 2, 2, 2, 1, 2, 2, 1, 1, 1, 2, 2, 2, 2, 1, 1, 1, 2, 2, 2, 2, 2, 2, 2, 2, 2, 2, 2, 2, 1, 1, 1, 1, 2, 4 ),
 ( 0.6520416950275925716, 0.6521563145716774423, 0.6521849694576987710, 0.6522136243437199887, 0.6522709341157624241, 0.6525001732039322766, 0.6529586513802718706, 0.6538756077329512806, 0.6543340859092908746, 0.6545633249974607271, 0.6546206347695031624, 0.6546492896555243801, 0.6546636170985350445, 0.6546779445415457088, 0.6547925640856305796, 0.6557095204383098785, 0.6566264767909891775, 0.6570849549673287715, 0.6571422647393712069, 0.6571565921823818712, 0.6571637559038872034, 0.6571709196253924246, 0.6571995745114136422, 0.6573141940554986240, 0.6575434331436683655, 0.6584603894963475534, 0.6593773458490268524, 0.6596065849371965939, 0.6596638947092390293, 0.6596782221522496936, 0.6596925495952603580, 0.6597212044812815757, 0.6598358240253664464, 0.6602943022017061514, 0.6612112585543855614, 0.6613258780984705432, 0.6613402055414812075, 0.6613545329844917608, 0.6613831878705129785, 0.6614404976425554139, 0.6616697367307252664, 0.6621282149070649714, 0.6625866930834045654, 0.6628159321715744179, 0.6630451712597442704, 0.6639621276124235694, 0.6648790839651028683, 0.6657960403177821673, 0.6662545184941217613, 0.6663118282661641967, 0.6663404831521855254, 0.6663476468736907465, 0.6663548105951960787, 0.6663691380382067431, 0.6664837575822916138, 0.6667129966704614663, 0.6676299530231408763, 0.6680884311994804703, 0.6682030507435654521, 0.6682603605156078874, 0.6683176702876503228, 0.6685469093758201753, 0.6694638657284994743, 0.6699223439048391793, 0.6701515829930090318, 0.6701659104360195851, 0.6701802378790302495, 0.6702088927650514671, 0.6702662025370939025, 0.6703808220811788843, 0.6712977784338580722, 0.6717562566101977772, 0.6719854956983676297, 0.6720428054704100651, 0.6720571329134206184, 0.6720607147741732845, 0.6720642966349259506, 0.6720714603564312828, 0.6721001152424525005, 0.6722147347865373712, 0.6731316911392165592, 0.6735901693155561532, 0.6738194084037260057, 0.6739340279478108764, 0.6739626828338320941, 0.6739698465553374263, 0.6739770102768426474, 0.6739913377198533118, 0.6740486474918957471, 0.6758825601972537900, 0.6767995165499328669, 0.6768138439929434202, 0.6768281714359540846, 0.6768568263219753023, 0.6769141360940176266, 0.6770287556381024974, 0.6772579947262722389, 0.6777164729026114998, 0.6781749510789508717, 0.6784041901671206132, 0.6786334292552902436, 0.6795503856079689875, 0.6796650051520537472, 0.6797796246961386180, 0.6800088637843082484, 0.6804673419606476203, 0.6809258201369869923, 0.6811550592251567338, 0.6812696787692414935, 0.6813269885412839288, 0.6813556434273051465, 0.6813699708703158109, 0.6813771345918210320, 0.6813842983133263642 ),
 .UNSPECIFIED. ) ;
#2867 = CARTESIAN_POINT ( 'NONE',  ( -13.49850325917753935, 64.94645159456099748, 0.4826294637078544225 ) ) ;
#2868 = ORIENTED_EDGE ( 'NONE', *, *, #3222, .F. ) ;
#2869 = CARTESIAN_POINT ( 'NONE',  ( -13.34768415857563895, 35.00084492118001123, 2.022211493481883338 ) ) ;
#2870 = ORIENTED_EDGE ( 'NONE', *, *, #7896, .F. ) ;
#2871 = CARTESIAN_POINT ( 'NONE',  ( 12.57096588966968476, 78.25114472168620239, 4.928957368016985363 ) ) ;
#2872 = DIRECTION ( 'NONE',  ( -0.000000000000000000, 1.000000000000000000, -0.000000000000000000 ) ) ;
#2873 = EDGE_CURVE ( 'NONE', #13703, #10105, #16524, .T. ) ;
#2874 = CARTESIAN_POINT ( 'NONE',  ( -11.71377142868683308, 31.68060524350620710, -6.712565316410540106 ) ) ;
#2875 = CARTESIAN_POINT ( 'NONE',  ( 10.57277106256930743, 72.74993520006962910, -8.398181679965585289 ) ) ;
#2876 = CARTESIAN_POINT ( 'NONE',  ( -4.171729424061787483, -18.66999999999999815, -12.83926296998457417 ) ) ;
#2877 = CARTESIAN_POINT ( 'NONE',  ( 13.49999999999999822, 69.27999999999997272, 4.386415899144237684 ) ) ;
#2878 = CARTESIAN_POINT ( 'NONE',  ( -13.44352697023783882, 52.97286464824527741, 1.235290049340939333 ) ) ;
#2879 = AXIS2_PLACEMENT_3D ( 'NONE', #15450, #6121, #2017 ) ;
#2880 = CARTESIAN_POINT ( 'NONE',  ( 3.636496289402157078, 44.03000000000000114, -11.19198476289190936 ) ) ;
#2881 = CARTESIAN_POINT ( 'NONE',  ( -10.92172942406179104, 67.23000000000000398, 7.935100905948387684 ) ) ;
#2882 = PLANE ( 'NONE',  #15753 ) ;
#2883 = CARTESIAN_POINT ( 'NONE',  ( 11.79460588130421250, 69.18643917531105103, 6.568504325302008340 ) ) ;
#2884 = CARTESIAN_POINT ( 'NONE',  ( 3.708203932499379185, 3.163974596215581414, -11.41267819554186858 ) ) ;
#2885 = CARTESIAN_POINT ( 'NONE',  ( 1.346677795875271366, 35.72842155251986895, 13.43267107845611896 ) ) ;
#2886 = CARTESIAN_POINT ( 'NONE',  ( 11.37500000000039613, -91.54062499999980673, -4.711679271993002516 ) ) ;
#2887 = CARTESIAN_POINT ( 'NONE',  ( -12.02303369154052426, 74.15637003178895270, 6.139850934852907116 ) ) ;
#2888 = CARTESIAN_POINT ( 'NONE',  ( -13.49205587446478027, 76.94592520882854103, 0.4631159351518623901 ) ) ;
#2889 = AXIS2_PLACEMENT_3D ( 'NONE', #8915, #3500, #3678 ) ;
#2890 = CARTESIAN_POINT ( 'NONE',  ( -4.171729424061791036, 0.5300000000000026912, 12.83926296998457239 ) ) ;
#2891 = CARTESIAN_POINT ( 'NONE',  ( -9.708203932499371192, 1.096025403784446350, 7.053423027509678533 ) ) ;
#2892 = DIRECTION ( 'NONE',  ( 0.000000000000000000, 0.000000000000000000, -1.000000000000000000 ) ) ;
#2893 = CARTESIAN_POINT ( 'NONE',  ( 9.520470885617717371, -3.269999999999995133, -6.917026985038131848 ) ) ;
#2894 = CARTESIAN_POINT ( 'NONE',  ( 11.76794919243112325, 49.42999999999999972, 1.441158131103945434E-15 ) ) ;
#2895 = CARTESIAN_POINT ( 'NONE',  ( 0.2252273365623476686, -18.34015606061350567, 15.45843899586301973 ) ) ;
#2896 = CARTESIAN_POINT ( 'NONE',  ( 2.138189944381242213, 36.10311857767973720, -13.49999999999999822 ) ) ;
#2897 = CARTESIAN_POINT ( 'NONE',  ( 12.36199458607823054, 75.23191100907908435, 5.426195953618915269 ) ) ;
#2898 = DIRECTION ( 'NONE',  ( 0.000000000000000000, 0.000000000000000000, -1.000000000000000000 ) ) ;
#2899 = CARTESIAN_POINT ( 'NONE',  ( 2.272985001014427788E-15, 35.17999999999998550, -12.37355403259654985 ) ) ;
#2900 = CARTESIAN_POINT ( 'NONE',  ( -11.99741742274050793, 41.15884529835775396, 6.204743281297112389 ) ) ;
#2901 = CARTESIAN_POINT ( 'NONE',  ( 2.445080149700053643E-15, 66.18000000000000682, -13.50000000000000000 ) ) ;
#2902 = CARTESIAN_POINT ( 'NONE',  ( 2.399255109878465575, 44.76621471937859553, 13.28788051155532912 ) ) ;
#2903 = B_SPLINE_CURVE_WITH_KNOTS ( 'NONE', 3,
 ( #12973, #3511, #14456, #11570, #1036, #8925, #14284, #6104, #14201, #2169, #12890, #13147, #2083, #15780, #7682, #7595, #16860, #4846, #778, #10250, #9190, #10169, #15517, #855, #8845, #17030, #943, #4935, #6185, #13061, #6444, #2425, #6354, #11739, #16944, #10335, #7775, #3690, #7508, #15690, #15604, #6266, #3596, #11653, #14539, #9009, #2343, #14366, #7858, #10421, #17117, #11486, #2254, #5022, #3429, #9103, #11829, #17207, #5117, #10509, #15871, #692, #17291, #17461, #9624, #13316, #9449, #10594, #6701, #9276, #7943, #13570, #14975, #3862, #6534, #11913, #1461, #2514, #14798, #1208, #5204, #16304, #5462, #2689, #1121, #15955, #8120, #14629, #6617, #2867, #16212, #2601, #11997, #17379, #13233, #12168, #5294, #4124, #10676, #9537, #16041, #3949, #12080, #9363, #14713, #6881, #8031, #13398, #1287, #5374, #12253, #10761, #13486, #16124, #4035, #1374, #6788, #148, #59, #10845, #14882, #2778, #8208, #5554, #10938, #4212, #14000, #4388, #9799, #1637, #7139, #16747, #6967, #15238, #4300, #12346, #15145, #12695, #13913, #7055, #1807, #4654, #582, #8646, #11200, #7221, #5730, #9975, #13824, #7309, #9712, #10062, #13739, #2956, #11112, #5992, #16484, #12435, #11375, #3042, #8474, #321, #1549, #1724, #238, #3226, #16576, #5644, #5817, #8384, #12608, #3135, #12525, #497, #11026, #409, #15412, #8297, #16397, #15056, #4481, #5904, #11283, #13654, #9890, #8560, #4567, #16660 ),
 .UNSPECIFIED., .F., .F.,
 ( 4, 2, 2, 2, 1, 1, 2, 2, 1, 2, 1, 2, 2, 1, 1, 2, 2, 2, 2, 1, 2, 2, 2, 2, 2, 2, 2, 2, 1, 1, 2, 2, 1, 1, 2, 2, 1, 1, 2, 2, 2, 2, 2, 1, 1, 2, 2, 2, 1, 2, 2, 1, 2, 2, 1, 1, 1, 2, 2, 1, 2, 2, 2, 2, 2, 2, 2, 2, 2, 2, 2, 1, 1, 1, 1, 2, 2, 1, 2, 2, 1, 1, 2, 2, 2, 2, 2, 2, 2, 2, 1, 2, 2, 1, 1, 2, 2, 2, 2, 2, 1, 1, 2, 2, 2, 2, 2, 2, 1, 2, 4 ),
 ( 0.2989785326016397571, 0.2998994589697745461, 0.3003599221538418851, 0.3005901537458756101, 0.3007052695418924171, 0.3007628274399008483, 0.3007772169144029561, 0.3007916063889050640, 0.3008203853379092796, 0.3026622380741786911, 0.3027197959721871223, 0.3027341854466892301, 0.3027413801839403118, 0.3027485749211913379, 0.3027773538701955536, 0.3028924696662123051, 0.3031227012582458635, 0.3035831644423129805, 0.3045040908104472699, 0.3046192066064640214, 0.3046767645044724526, 0.3047343224024808284, 0.3049645539945143868, 0.3054250171785815038, 0.3063459435467157932, 0.3065761751387493517, 0.3066337330367577274, 0.3066625119857619430, 0.3066912909347661587, 0.3068064067307829101, 0.3072668699148500826, 0.3081877962829843720, 0.3084180278750179860, 0.3085331436710347375, 0.3085907015690431687, 0.3086050910435452210, 0.3086194805180473288, 0.3086482594670515445, 0.3091087226511187169, 0.3100296490192530618, 0.3104901122033202343, 0.3105188911523243944, 0.3105476701013286100, 0.3106052279993369858, 0.3107203437953537928, 0.3109505753873874068, 0.3118715017555217517, 0.3123319649395889241, 0.3124470807356057311, 0.3124758596846099468, 0.3125046386336141624, 0.3125621965316225381, 0.3127924281236560966, 0.3137133544917904415, 0.3141738176758576140, 0.3144040492678912280, 0.3144328282168954436, 0.3144472176913974959, 0.3144616071658996037, 0.3145191650639080350, 0.3146342808599247864, 0.3155552072280591314, 0.3160156704121263038, 0.3162459020041598623, 0.3163610178001766693, 0.3164185756981850450, 0.3164761335961934763, 0.3173970599643277657, 0.3183179863324621106, 0.3183467652814663262, 0.3183611547559684340, 0.3183755442304705419, 0.3184331021284789176, 0.3185482179244957246, 0.3187784495165293386, 0.3192389127005965666, 0.3201598390687310225, 0.3202749548647478295, 0.3203037338137519896, 0.3203181232882540974, 0.3203325127627562052, 0.3203900706607645810, 0.3206203022527980839, 0.3210807654368651454, 0.3220016918049992127, 0.3222319233970327157, 0.3224621549890662742, 0.3229226181731332801, 0.3238435445412673475, 0.3240737761333008504, 0.3241888919293176574, 0.3242176708783218175, 0.3242320603528239253, 0.3242464498273260332, 0.3243040077253344089, 0.3247644709094015258, 0.3256853972775357042, 0.3261458604616027657, 0.3261602499361048735, 0.3261746394106069813, 0.3262034183596111969, 0.3262609762576195727, 0.3263760920536363241, 0.3266063236456698826, 0.3275272500138040055, 0.3279877131978710669, 0.3281028289938878184, 0.3281316079428920340, 0.3281603868918961942, 0.3282179447899046254, 0.3284481763819381284 ),
 .UNSPECIFIED. ) ;
#2904 = CARTESIAN_POINT ( 'NONE',  ( 8.343458848123580296, 58.98000000000000398, 11.48378591275253768 ) ) ;
#2905 = CARTESIAN_POINT ( 'NONE',  ( -24.73863375370588003, 5.918584287042170544, -8.000000000000282441 ) ) ;
#2906 = EDGE_CURVE ( 'NONE', #17443, #16027, #15981, .T. ) ;
#2907 = CARTESIAN_POINT ( 'NONE',  ( 6.767892274116773521, 80.93000000001259764, -11.68099457092376348 ) ) ;
#2908 = CARTESIAN_POINT ( 'NONE',  ( -10.12981325033382340, 49.58606605476560247, -8.923950245100398249 ) ) ;
#2909 = CARTESIAN_POINT ( 'NONE',  ( 11.56754221458070298, 63.17051984811690346, 6.960026861118096875 ) ) ;
#2910 = CARTESIAN_POINT ( 'NONE',  ( 12.83702738905192398, 42.27686750378746439, 4.271642589196766870 ) ) ;
#2911 = CARTESIAN_POINT ( 'NONE',  ( 5.936052360656044691, 48.96357924273701911, -12.12490342414647593 ) ) ;
#2912 = ORIENTED_EDGE ( 'NONE', *, *, #12292, .F. ) ;
#2913 = CARTESIAN_POINT ( 'NONE',  ( -3.636496289402155746, 75.53000000000000114, 11.19198476289190936 ) ) ;
#2914 = CARTESIAN_POINT ( 'NONE',  ( -1.732050807568877859, 0.000000000000000000, -18.99999999999999645 ) ) ;
#2915 = CARTESIAN_POINT ( 'NONE',  ( 4.711679271994910323, -3.121874999999992184, -11.37499999999960387 ) ) ;
#2916 = CARTESIAN_POINT ( 'NONE',  ( 8.343458848123578520, 8.980000000000011084, 11.48378591275254124 ) ) ;
#2917 = VERTEX_POINT ( 'NONE', #84 ) ;
#2918 = CARTESIAN_POINT ( 'NONE',  ( -8.698957838002245424, 43.51485979879910815, -10.32366908839676078 ) ) ;
#2919 = CYLINDRICAL_SURFACE ( 'NONE', #16696, 13.50000000000000000 ) ;
#2920 = CARTESIAN_POINT ( 'NONE',  ( 11.66807071203169777, 60.68264838426821939, -6.791431104833153043 ) ) ;
#2921 = CARTESIAN_POINT ( 'NONE',  ( -13.49999999999999822, 11.77999999999999758, -4.386415899144240349 ) ) ;
#2922 = CARTESIAN_POINT ( 'NONE',  ( 0.000000000000000000, 73.00000000000001421, 0.000000000000000000 ) ) ;
#2923 = CARTESIAN_POINT ( 'NONE',  ( 13.44884314945179682, 66.38927782166076952, 1.174156769367327824 ) ) ;
#2924 = CARTESIAN_POINT ( 'NONE',  ( 3.171349303842611711, 56.79407181424019768, 13.12227985861226109 ) ) ;
#2925 = CARTESIAN_POINT ( 'NONE',  ( -7.272992578804307939, 56.47999999999998977, -10.01041549318726886 ) ) ;
#2926 = CARTESIAN_POINT ( 'NONE',  ( -9.520470885617717371, 63.23000000000001108, 6.917026985038133624 ) ) ;
#2927 = CARTESIAN_POINT ( 'NONE',  ( -12.25285257643324321, 47.13773527728996271, 5.669290189831918347 ) ) ;
#2928 = DIRECTION ( 'NONE',  ( 0.000000000000000000, 0.000000000000000000, 1.000000000000000000 ) ) ;
#2929 = DIRECTION ( 'NONE',  ( 0.000000000000000000, 1.000000000000000000, 0.000000000000000000 ) ) ;
#2930 = CARTESIAN_POINT ( 'NONE',  ( 8.257394697130328254, 30.86552653227584742, -10.68051812031342251 ) ) ;
#2931 = ADVANCED_FACE ( 'NONE', ( #1491 ), #6725, .T. ) ;
#2932 = CARTESIAN_POINT ( 'NONE',  ( -2.134337778213805326, 56.60326167549609266, 13.33023129177848887 ) ) ;
#2933 = CARTESIAN_POINT ( 'NONE',  ( -11.37500000000000000, -58.27499999999986358, -9.545674412382054647E-13 ) ) ;
#2934 = LINE ( 'NONE', #16286, #13446 ) ;
#2935 = AXIS2_PLACEMENT_3D ( 'NONE', #2156, #7580, #12959 ) ;
#2936 = CARTESIAN_POINT ( 'NONE',  ( 13.29699880966072278, 33.34798608968654321, 2.332353922266759305 ) ) ;
#2937 = DIRECTION ( 'NONE',  ( -0.000000000000000000, 1.000000000000000000, -0.000000000000000000 ) ) ;
#2938 = CARTESIAN_POINT ( 'NONE',  ( 0.1174797757853172780, 40.17577724366387315, -13.49956142739842058 ) ) ;
#2939 = CARTESIAN_POINT ( 'NONE',  ( -7.272992578804310604, 22.38000000000000966, 10.01041549318726709 ) ) ;
#2940 = EDGE_LOOP ( 'NONE', ( #4125, #7707, #14866, #16925 ) ) ;
#2941 = CARTESIAN_POINT ( 'NONE',  ( -2.239153631970620673, 62.59948832305353505, 13.31301680066964543 ) ) ;
#2942 = ORIENTED_EDGE ( 'NONE', *, *, #13823, .T. ) ;
#2943 = CARTESIAN_POINT ( 'NONE',  ( -13.45392095391353671, 40.96936140205911414, 1.136027132915432114 ) ) ;
#2944 = CARTESIAN_POINT ( 'NONE',  ( 7.272992578804308828, -13.02000000000000313, 10.01041549318726709 ) ) ;
#2945 = CARTESIAN_POINT ( 'NONE',  ( 1.561832610794586740E-12, -28.06249999999995381, -18.62500000000000000 ) ) ;
#2946 = CARTESIAN_POINT ( 'NONE',  ( -11.20488271874176078, 44.21300015732045097, 7.529980452644597477 ) ) ;
#2947 = B_SPLINE_CURVE_WITH_KNOTS ( 'NONE', 3,
 ( #4802, #2379, #7814, #10204, #3551, #895, #15557, #5067, #7548, #13187, #7637, #11780, #9052, #13098, #6222, #8882, #14406, #3468, #10289, #984, #12926 ),
 .UNSPECIFIED., .F., .F.,
 ( 4, 2, 2, 2, 1, 2, 2, 2, 2, 1, 1, 4 ),
 ( 0.000000000000000000, 0.001230814438799202265, 0.001846221658198803290, 0.002000073463048703763, 0.002153925267898604452, 0.002461628877598403230, 0.003692443316397600508, 0.003846295121247500330, 0.003923221023672450458, 0.004000146926097401454, 0.004307850535797202833, 0.004923257755196806459 ),
 .UNSPECIFIED. ) ;
#2948 = DIRECTION ( 'NONE',  ( 0.000000000000000000, -1.000000000000000000, 0.000000000000000000 ) ) ;
#2949 = CARTESIAN_POINT ( 'NONE',  ( 10.92172942406179104, 30.72999999999999332, -7.935100905948385908 ) ) ;
#2950 = PRODUCT ( 'Spring', 'Spring', '', ( #3873 ) ) ;
#2951 = CARTESIAN_POINT ( 'NONE',  ( -18.62499999999935341, -49.98437499999987210, -7.714727599200458030 ) ) ;
#2952 = ADVANCED_FACE ( 'NONE', ( #9560 ), #14910, .T. ) ;
#2953 = CARTESIAN_POINT ( 'NONE',  ( -10.07108133119379012, 67.58295566904861573, -8.990215881721550062 ) ) ;
#2954 = CARTESIAN_POINT ( 'NONE',  ( 13.16986379960055409, -44.78124999999987921, -13.16986379959834430 ) ) ;
#2955 = CARTESIAN_POINT ( 'NONE',  ( 11.54962138675810479, 54.69070229437127750, -6.989731339562734291 ) ) ;
#2956 = CARTESIAN_POINT ( 'NONE',  ( -5.888583767921062417, 64.39455096188707728, -12.14803002262569720 ) ) ;
#2957 = VERTEX_POINT ( 'NONE', #5930 ) ;
#2958 = CARTESIAN_POINT ( 'NONE',  ( -12.72183143979101416, 35.09323451362223523, 4.520332688420920952 ) ) ;
#2959 = ORIENTED_EDGE ( 'NONE', *, *, #14702, .T. ) ;
#2960 = CARTESIAN_POINT ( 'NONE',  ( 13.25352574315592058, 78.33850325101057877, 2.596262599255617420 ) ) ;
#2961 = CARTESIAN_POINT ( 'NONE',  ( -10.99999999999979394, 7.773118517290098950, -15.58845726812003996 ) ) ;
#2962 = CARTESIAN_POINT ( 'NONE',  ( 7.500000000000000888, -27.79702113870390789, -1.010069558262736145 ) ) ;
#2963 = CARTESIAN_POINT ( 'NONE',  ( 5.943805720458234632, 72.96327358916208539, -12.12110495732162541 ) ) ;
#2964 = CARTESIAN_POINT ( 'NONE',  ( 12.01373065778716231, 78.65715868066507710, -6.159954580827336379 ) ) ;
#2965 = CARTESIAN_POINT ( 'NONE',  ( 4.171729424061791924, -15.96999999999999886, -12.83926296998457239 ) ) ;
#2966 = VECTOR ( 'NONE', #14736, 1000.000000000000000 ) ;
#2967 = CARTESIAN_POINT ( 'NONE',  ( 8.343458848123578520, 65.97999999999997556, 11.48378591275254124 ) ) ;
#2968 = CARTESIAN_POINT ( 'NONE',  ( -13.49277924355403613, 52.91293775321170756, -0.4922678860690162250 ) ) ;
#2969 = CARTESIAN_POINT ( 'NONE',  ( -3.636496289402155746, 42.53000000000000114, 11.19198476289190936 ) ) ;
#2970 = CARTESIAN_POINT ( 'NONE',  ( -13.49999999999999822, 61.07999999999999119, 4.386415899144235908 ) ) ;
#2971 = CARTESIAN_POINT ( 'NONE',  ( -15.43494339453330255, 7.854708401161940579, -10.68872673103606807 ) ) ;
#2972 = CARTESIAN_POINT ( 'NONE',  ( 3.530559298853932049, 68.80696058099172774, 13.03017551344940550 ) ) ;
#2973 = CARTESIAN_POINT ( 'NONE',  ( 1.900613283894441619, 3.237093173895313480, -12.00000000000002665 ) ) ;
#2974 = EDGE_CURVE ( 'NONE', #2583, #13643, #5827, .T. ) ;
#2975 = CARTESIAN_POINT ( 'NONE',  ( 2.000520122481862502E-14, 73.67999999999999261, 13.50000000000000000 ) ) ;
#2976 = CARTESIAN_POINT ( 'NONE',  ( 18.62499999999935341, -56.15937499999989058, 7.714727599200469577 ) ) ;
#2977 = CARTESIAN_POINT ( 'NONE',  ( -8.440553202013695966, 74.35714477797125710, 10.53601240182882037 ) ) ;
#2978 = CARTESIAN_POINT ( 'NONE',  ( -9.366007952159224104, 76.54695510398188674, -9.722646867579905816 ) ) ;
#2979 = CARTESIAN_POINT ( 'NONE',  ( 2.894739590358088936E-06, 0.6800804143413337055, 13.49999999999938360 ) ) ;
#2980 = PLANE ( 'NONE',  #162 ) ;
#2981 = CARTESIAN_POINT ( 'NONE',  ( 7.347880794884121708E-16, -22.00000000000000000, 6.000000000000001776 ) ) ;
#2982 = CARTESIAN_POINT ( 'NONE',  ( -11.76794919243112325, -4.919999999999999041, 3.823638476888994386 ) ) ;
#2983 = CARTESIAN_POINT ( 'NONE',  ( 9.520470885617717371, 46.73000000000000398, -6.917026985038131848 ) ) ;
#2984 = CARTESIAN_POINT ( 'NONE',  ( 4.171729424061791924, -16.96999999999999886, -12.83926296998457239 ) ) ;
#2985 = CARTESIAN_POINT ( 'NONE',  ( -2.056889372791192105, 32.60599326084160765, 13.34339756607785965 ) ) ;
#2986 = CARTESIAN_POINT ( 'NONE',  ( 13.06624678191117894, 75.55090238563390415, -3.394585794078206487 ) ) ;
#2987 = CARTESIAN_POINT ( 'NONE',  ( 17.50831196659380140, 3.710240846040484935E-14, -6.047149036516558773 ) ) ;
#2988 = VECTOR ( 'NONE', #13123, 1000.000000000000000 ) ;
#2989 = CARTESIAN_POINT ( 'NONE',  ( -12.47701956898900910, 41.11767325390844263, 5.155734636392532266 ) ) ;
#2990 = CARTESIAN_POINT ( 'NONE',  ( 6.930981503973903557, 51.92345320045085799, -11.59790771992309821 ) ) ;
#2991 = CARTESIAN_POINT ( 'NONE',  ( 0.000000000000000000, 80.93000000000000682, -13.50000000000000000 ) ) ;
#2992 = EDGE_CURVE ( 'NONE', #13643, #2583, #8587, .T. ) ;
#2993 = DIRECTION ( 'NONE',  ( 1.000000000000000000, 0.000000000000000000, 0.000000000000000000 ) ) ;
#2994 = CARTESIAN_POINT ( 'NONE',  ( 1.653273178848926472E-15, 80.93000000000000682, 13.50000000000000000 ) ) ;
#2995 = LINE ( 'NONE', #9842, #16830 ) ;
#2996 = CARTESIAN_POINT ( 'NONE',  ( 8.859641085343996636, 63.02212108781364464, 10.19330108810972924 ) ) ;
#2997 = CARTESIAN_POINT ( 'NONE',  ( 10.69513479019918911, 42.11700743034955252, 8.237987836516895257 ) ) ;
#2998 = CARTESIAN_POINT ( 'NONE',  ( -18.02297152527630786, 8.055324227812098670, -0.3502263562677673248 ) ) ;
#2999 = CARTESIAN_POINT ( 'NONE',  ( -11.76794919243112325, 22.08000000000000540, 3.823638476888994386 ) ) ;
#3000 = ORIENTED_EDGE ( 'NONE', *, *, #11955, .T. ) ;
#3001 = CARTESIAN_POINT ( 'NONE',  ( 11.76794919243112680, 73.58000000000001251, -3.823638476888993942 ) ) ;
#3002 = DIRECTION ( 'NONE',  ( -0.000000000000000000, 1.000000000000000000, -0.000000000000000000 ) ) ;
#3003 = CARTESIAN_POINT ( 'NONE',  ( -11.37500000000039613, -59.31562499999985505, 4.711679271993001628 ) ) ;
#3004 = CARTESIAN_POINT ( 'NONE',  ( 13.49999999999999822, 6.279999999999996696, 4.386415899144237684 ) ) ;
#3005 = ORIENTED_EDGE ( 'NONE', *, *, #14767, .F. ) ;
#3006 = CARTESIAN_POINT ( 'NONE',  ( -4.007469125189920156, 43.32409381421197025, -12.89150143208222765 ) ) ;
#3007 = CARTESIAN_POINT ( 'NONE',  ( -7.499999999999997335, 104.6873333394686796, 9.035253535952435300 ) ) ;
#3008 = CARTESIAN_POINT ( 'NONE',  ( 12.99308620456710806, 60.56095136765374320, -3.664675452714382775 ) ) ;
#3009 = CARTESIAN_POINT ( 'NONE',  ( 10.92172942406178926, 4.129999999999994564, 7.935100905948385908 ) ) ;
#3010 = CARTESIAN_POINT ( 'NONE',  ( -18.62500000000000000, -8.324999999999979750, -1.562973063126292555E-12 ) ) ;
#3011 = CARTESIAN_POINT ( 'NONE',  ( 3.786209671971815016, 65.81577437060603586, 12.96002889484262965 ) ) ;
#3012 = CARTESIAN_POINT ( 'NONE',  ( 10.28852882370732935, 57.09439556068322474, 8.746997244907646518 ) ) ;
#3013 = CARTESIAN_POINT ( 'NONE',  ( -7.576616670048093940E-16, 60.67999999999998550, 12.37355403259654985 ) ) ;
#3014 = CARTESIAN_POINT ( 'NONE',  ( 10.92172942406179104, 35.72999999999999687, -7.935100905948385908 ) ) ;
#3015 = CARTESIAN_POINT ( 'NONE',  ( -7.576616670048093940E-16, 66.67999999999997840, 12.37355403259654985 ) ) ;
#3016 = CARTESIAN_POINT ( 'NONE',  ( -13.49258962402246098, 46.94538227618738091, 0.4474236191536023477 ) ) ;
#3017 = CARTESIAN_POINT ( 'NONE',  ( 7.545661582016999880, 45.89709249710414696, -11.19442553811792251 ) ) ;
#3018 = CYLINDRICAL_SURFACE ( 'NONE', #9684, 13.50000000000000000 ) ;
#3019 = FILL_AREA_STYLE_COLOUR ( '', #3840 ) ;
#3020 = CARTESIAN_POINT ( 'NONE',  ( 3.634147496961807722, 31.04944686732046222, -13.02236486152032491 ) ) ;
#3021 = CARTESIAN_POINT ( 'NONE',  ( -11.85687157084362120, 9.999999999999998224, -2.107649565213920440 ) ) ;
#3022 = CARTESIAN_POINT ( 'NONE',  ( -8.043339635997654113, -93.65624999999977263, 8.043339635996302306 ) ) ;
#3023 = CARTESIAN_POINT ( 'NONE',  ( -4.171729424061787483, 39.32999999999999829, -12.83926296998457417 ) ) ;
#3024 = CARTESIAN_POINT ( 'NONE',  ( 3.999863251508507744, 32.82381939080141819, 12.89392482267520634 ) ) ;
#3025 = FACE_OUTER_BOUND ( 'NONE', #5026, .T. ) ;
#3026 = CARTESIAN_POINT ( 'NONE',  ( 2.003101852233307056, 40.10816637432754561, -13.35920704381847557 ) ) ;
#3027 = CARTESIAN_POINT ( 'NONE',  ( -9.520470885617717371, 22.23000000000000043, 6.917026985038133624 ) ) ;
#3028 = ORIENTED_EDGE ( 'NONE', *, *, #1488, .F. ) ;
#3029 = CARTESIAN_POINT ( 'NONE',  ( -11.98320029393328490, 62.16226028446121887, 6.301581060576362248 ) ) ;
#3030 = ORIENTED_EDGE ( 'NONE', *, *, #2316, .F. ) ;
#3031 = CARTESIAN_POINT ( 'NONE',  ( -11.76794919243112325, -16.92000000000000526, 3.823638476888994386 ) ) ;
#3032 = CARTESIAN_POINT ( 'NONE',  ( 7.714727599200456254, -27.02187499999995524, -18.62499999999935341 ) ) ;
#3033 = CARTESIAN_POINT ( 'NONE',  ( -10.82450696210587360, 44.23580785916440306, 8.068722966871488822 ) ) ;
#3034 = DIRECTION ( 'NONE',  ( 0.5000000000000066613, 0.000000000000000000, -0.8660254037844347108 ) ) ;
#3035 = EDGE_CURVE ( 'NONE', #309, #5991, #2681, .T. ) ;
#3036 = CARTESIAN_POINT ( 'NONE',  ( 6.750017152462248760, 29.92926152634062475, 11.69133304809444773 ) ) ;
#3037 = CARTESIAN_POINT ( 'NONE',  ( -8.691771469529815392E-16, 46.67999999999999972, 14.19474002721660355 ) ) ;
#3038 = CARTESIAN_POINT ( 'NONE',  ( -5.043317043880707118, 46.36194157942755112, -12.52473711853716409 ) ) ;
#3039 = CARTESIAN_POINT ( 'NONE',  ( -3.069954153749930637, 67.29026836399954448, -13.14679252126118492 ) ) ;
#3040 = CARTESIAN_POINT ( 'NONE',  ( -13.16986379960055409, -69.75624999999980957, 13.16986379959834252 ) ) ;
#3041 = CARTESIAN_POINT ( 'NONE',  ( -7.499999999999998224, -8.000000000000000000, 9.367496997597587693 ) ) ;
#3042 = CARTESIAN_POINT ( 'NONE',  ( -5.372399846363435927, 64.37448310051588862, -12.38690699972042530 ) ) ;
#3044 = VERTEX_POINT ( 'NONE', #522 ) ;
#3043 = MANIFOLD_SOLID_BREP ( 'Boss-Extrude4', #10309 ) ;
#3045 = CARTESIAN_POINT ( 'NONE',  ( 16.03410433562979520, 8.027996319639559175, -8.458421099448731439 ) ) ;
#3046 = CARTESIAN_POINT ( 'NONE',  ( -11.71399375460170766, 34.68062007852038420, -6.712177567382903831 ) ) ;
#3047 = CARTESIAN_POINT ( 'NONE',  ( 8.043339635996300530, -31.21874999999992539, 8.043339635997654113 ) ) ;
#3048 = CIRCLE ( 'NONE', #8726, 13.50000000000000000 ) ;
#3049 = ORIENTED_EDGE ( 'NONE', *, *, #17329, .F. ) ;
#3050 = CARTESIAN_POINT ( 'NONE',  ( 12.20032402202371991, 78.21732329587429433, 5.797904856266742790 ) ) ;
#3051 = DIRECTION ( 'NONE',  ( 0.000000000000000000, 0.000000000000000000, -1.000000000000000000 ) ) ;
#3052 = CARTESIAN_POINT ( 'NONE',  ( 7.500000000000003553, -27.54571194363308706, 3.584587286925209337 ) ) ;
#3053 = CARTESIAN_POINT ( 'NONE',  ( 13.40079223352167759, 72.37267490479835885, 1.638534314007722870 ) ) ;
#3054 = CARTESIAN_POINT ( 'NONE',  ( 4.952149856071437206, 79.00137556925825777, -12.55891152037733249 ) ) ;
#3055 = ADVANCED_FACE ( 'NONE', ( #347 ), #7486, .F. ) ;
#3056 = CARTESIAN_POINT ( 'NONE',  ( -8.343458848123582072, -17.62000000000000099, 11.48378591275254124 ) ) ;
#3057 = CARTESIAN_POINT ( 'NONE',  ( -10.92172942406179104, 65.22999999999998977, 7.935100905948387684 ) ) ;
#3058 = CARTESIAN_POINT ( 'NONE',  ( -13.47878953293021631, 52.90389950247480044, -0.7564620949284726059 ) ) ;
#3059 = CARTESIAN_POINT ( 'NONE',  ( 11.76794919243112680, 37.57999999999999829, -3.823638476888993942 ) ) ;
#3060 = CARTESIAN_POINT ( 'NONE',  ( 2.279995255611139653E-15, -17.82000000000000028, -12.37355403259654985 ) ) ;
#3061 = CARTESIAN_POINT ( 'NONE',  ( -13.49999999999999822, 58.07999999999999119, 4.386415899144235908 ) ) ;
#3062 = COLOUR_RGB ( '',0.7921568627450980005, 0.8196078431372548767, 0.9333333333333333481 ) ;
#3063 = CARTESIAN_POINT ( 'NONE',  ( -7.272992578804310604, -4.620000000000000995, 10.01041549318726709 ) ) ;
#3064 = CARTESIAN_POINT ( 'NONE',  ( 11.17437184405764228, 69.14511185220105460, 7.575987940921537600 ) ) ;
#3065 = CARTESIAN_POINT ( 'NONE',  ( 1.509281292405760415E-13, 1.813974596215571777, 12.00000000000000000 ) ) ;
#3066 = CARTESIAN_POINT ( 'NONE',  ( 0.000000000000000000, 80.93000000000000682, 0.000000000000000000 ) ) ;
#3067 = CARTESIAN_POINT ( 'NONE',  ( -7.714727599197334307, -79.05312499999985221, -18.62500000000064659 ) ) ;
#3068 = CARTESIAN_POINT ( 'NONE',  ( -12.80823760898952024, 73.77596097351039361, -4.279531554935352311 ) ) ;
#3069 =( BOUNDED_SURFACE ( )  B_SPLINE_SURFACE ( 3, 2, ( 
 ( #11395, #257, #11218, #16680, #9995, #9820, #3243, #8666, #16767, #9642, #16416, #10166, #8921, #15686, #4760, #2080, #10417, #3426, #7423, #14198, #14363, #2339, #15600, #3593, #15514, #11824, #10247, #852, #10080, #3340, #6263, #14111, #1996, #4675, #7679, #11567, #15431, #12803, #6441, #9005, #8755, #13058, #688, #940, #6101, #11482, #16941, #16857, #12886, #2251, #6351, #7505, #8841, #775, #11735, #13143, #6181, #14452, #14280, #4843, #3508, #2166, #7591, #17113, #11650, #12970, #17027, #4931, #5018, #10332, #15775, #3686, #9099, #7772, #1030, #16036, #8205, #15867, #6697, #13228, #3774, #6614, #4120, #5370, #15952, #10757, #14708, #17456, #17288, #3944, #9187, #11994, #16120, #13567, #17376, #6878, #12164 ),
 ( #14793, #14535, #10505, #2420, #1283, #55, #7853, #4031, #3858, #9445, #2597, #2685, #5200, #9359, #1117, #5290, #8116, #1458, #10672, #17204, #5459, #6531, #9272, #12077, #13482, #11909, #10590, #14624, #1370, #10842, #2510, #7940, #13312, #14878, #2774, #5112, #6785, #1203, #8026, #13394, #16209, #9534, #5727, #11198, #10935, #8295, #4297, #9797, #5901, #11023, #2954, #16302, #9970, #2863, #11109, #12523, #16482, #6965, #1635, #15143, #16657, #1722, #407, #235, #4386, #5814, #12343, #9710, #494, #16395, #14973, #15054, #4479, #15318, #3040, #16574, #5641, #1891, #318, #8471, #146, #4209, #13821, #9622, #13652, #12251, #15235, #7052, #5552, #1546, #13996, #9885, #8382, #3131, #13737, #8556, #12432 ),
 ( #7135, #13909, #1804, #7218, #12605, #11280, #4564, #3221, #8643, #17093, #16921, #4737, #5989, #11544, #14087, #4913, #14258, #8729, #1974, #10057, #8987, #3489, #7398, #7572, #14176, #8818, #666, #6163, #15756, #11371, #2148, #3315, #16743, #2061, #11718, #12778, #5000, #4823, #10141, #4651, #10225, #6077, #10311, #12949, #11457, #16833, #15409, #14344, #8904, #15493, #833, #7485, #12866, #3404, #15580, #3666, #755, #6244, #11630, #17005, #15665, #10399, #3574, #2232, #7662, #13039, #921, #6329, #9078, #14431, #7306, #12691, #579, #14608, #9515, #14777, #15847, #11893, #9343, #17439, #1011, #13122, #6422, #3926, #2667, #11805, #7837, #17183, #33, #5439, #10826, #14692, #5094, #17358, #14516, #1267, #2579 ),
 ( #10486, #10740, #16188, #4100, #5271, #5180, #3754, #5353, #12144, #9168, #2402, #13210, #1097, #1350, #8098, #8011, #13464, #7922, #7748, #2320, #9255, #6679, #15933, #16104, #6512, #13296, #10656, #17268, #10572, #3839, #4014, #1186, #2490, #12062, #9428, #6596, #11976, #16019, #13378, #6766, #125, #1705, #12324, #4369, #13720, #301, #10915, #1438, #1619, #11499, #14954, #11093, #12234, #8363, #16284, #6945, #2933, #7443, #7036, #8187, #13548, #3358, #4191, #13636, #14129, #15449, #16465, #8774, #12414, #2755, #14860, #4280, #13807, #11004, #390, #9604, #5711, #9778, #217, #16875, #5623, #11180, #15124, #4780, #7118, #12505, #6856, #1529, #16375, #5531, #3022, #2844, #5796, #9690, #8453, #16555, #4462 ),
 ( #8275, #15039, #9867, #2016, #12822, #709, #6119, #15710, #2442, #9028, #3445, #8862, #15887, #16962, #10183, #4864, #10267, #12906, #13076, #15534, #3705, #7874, #17309, #2186, #9122, #14214, #790, #9207, #3527, #7793, #8942, #11586, #873, #7699, #6463, #13164, #14300, #3795, #6549, #12990, #2360, #1051, #2099, #13251, #11928, #14559, #10524, #962, #14472, #7614, #11848, #3614, #1138, #6200, #6284, #10441, #11672, #17047, #7526, #4953, #10356, #15619, #14384, #2273, #17223, #6374, #11758, #17134, #5044, #15800, #5133, #13415, #17395, #171, #1223, #2798, #12185, #1305, #15975, #9294, #13590, #2886, #6989, #8137, #8048, #6636, #8229, #14994, #2534, #3878, #14646, #8318, #13673, #1570, #77, #7962, #2708 ),
 ( #16142, #4141, #13332, #12015, #14729, #13502, #16326, #3968, #6719, #5311, #12364, #10694, #4052, #5482, #9466, #16060, #12097, #1392, #9644, #10864, #16232, #9380, #14813, #9554, #2618, #17479, #10958, #5393, #10778, #6807, #14904, #5222, #1484, #6901, #12274, #10608, #5576, #4233, #5666, #16418, #13932, #9730, #15076, #7425, #3245, #7159, #11046, #2976, #1999, #16682, #4320, #8668, #8406, #14025, #258, #13758, #12544, #1658, #8494, #4589, #1914, #9823, #7073, #15168, #7333, #8757, #341, #10082, #9909, #3067, #12457, #4502, #5750, #15344, #7242, #11134, #16507, #4412, #12717, #1826, #13845, #516, #431, #1747, #5837, #16595, #14113, #11220, #12628, #15256, #3154, #8581, #4677, #5925, #11304, #9996, #603 ),
 ( #6014, #11397, #16769, #15433, #3343, #8844, #6184, #13060, #4845, #15603, #11828, #10249, #11569, #5115, #7594, #3510, #9102, #16943, #6353, #12888, #8923, #1034, #14282, #15516, #2168, #5021, #10508, #6265, #11738, #777, #2423, #854, #9008, #690, #11484, #14365, #4763, #10168, #12805, #15778, #12972, #6103, #3428, #14538, #17115, #16859, #3689, #14200, #14455, #2082, #7507, #11652, #17029, #4934, #10420, #2342, #10334, #15688, #3595, #7774, #3777, #2253, #15870, #7681, #942, #13146, #6443, #17206, #9189, #17460, #15954, #9275, #17290, #1373, #6699, #3861, #5373, #10675, #5293, #7942, #14712, #14881, #1120, #10760, #14628, #6533, #16040, #16211, #16123, #13315, #4034, #13397, #9448, #2513, #2600, #11912, #3948 ) ),
 .UNSPECIFIED., .T., .F., .F. ) 
 B_SPLINE_SURFACE_WITH_KNOTS ( ( 4, 3, 4 ),
 ( 3, 2, 2, 2, 2, 2, 2, 2, 2, 2, 2, 2, 2, 2, 2, 2, 2, 2, 2, 2, 2, 2, 2, 2, 2, 2, 2, 2, 2, 2, 2, 2, 2, 2, 2, 2, 2, 2, 2, 2, 2, 2, 2, 2, 2, 2, 2, 2, 3 ),
 ( 0.000000000000000000, 0.5000000000000000000, 1.000000000000000000 ),
 ( 0.000000000000000000, 0.02083333333333333218, 0.04166666666666666435, 0.06250000000000000000, 0.08333333333333332871, 0.1041666666666666713, 0.1250000000000000000, 0.1458333333333333426, 0.1666666666666666574, 0.1875000000000000000, 0.2083333333333333426, 0.2291666666666666574, 0.2500000000000000000, 0.2708333333333333148, 0.2916666666666666852, 0.3125000000000000000, 0.3333333333333333148, 0.3541666666666666852, 0.3750000000000000000, 0.3958333333333333148, 0.4166666666666666852, 0.4375000000000000000, 0.4583333333333333148, 0.4791666666666666852, 0.5000000000000000000, 0.5208333333333333703, 0.5416666666666666297, 0.5625000000000000000, 0.5833333333333333703, 0.6041666666666666297, 0.6250000000000000000, 0.6458333333333333703, 0.6666666666666666297, 0.6875000000000000000, 0.7083333333333333703, 0.7291666666666666297, 0.7500000000000000000, 0.7708333333333333703, 0.7916666666666666297, 0.8125000000000000000, 0.8333333333333333703, 0.8541666666666666297, 0.8750000000000000000, 0.8958333333333333703, 0.9166666666666666297, 0.9375000000000000000, 0.9583333333333333703, 0.9791666666666666297, 1.000000000000000000 ),
 .UNSPECIFIED. ) 
 GEOMETRIC_REPRESENTATION_ITEM ( )  RATIONAL_B_SPLINE_SURFACE ( (
 ( 1.000000000000000000, 0.9238795325112867385, 1.000000000000000000, 0.9238795325112867385, 1.000000000000000000, 0.9238795325112867385, 1.000000000000000000, 0.9238795325112867385, 1.000000000000000000, 0.9238795325112867385, 1.000000000000000000, 0.9238795325112867385, 1.000000000000000000, 0.9238795325112867385, 1.000000000000000000, 0.9238795325112867385, 1.000000000000000000, 0.9238795325112867385, 1.000000000000000000, 0.9238795325112867385, 1.000000000000000000, 0.9238795325112867385, 1.000000000000000000, 0.9238795325112867385, 1.000000000000000000, 0.9238795325112867385, 1.000000000000000000, 0.9238795325112867385, 1.000000000000000000, 0.9238795325112867385, 1.000000000000000000, 0.9238795325112867385, 1.000000000000000000, 0.9238795325112867385, 1.000000000000000000, 0.9238795325112867385, 1.000000000000000000, 0.9238795325112867385, 1.000000000000000000, 0.9238795325112867385, 1.000000000000000000, 0.9238795325112867385, 1.000000000000000000, 0.9238795325112867385, 1.000000000000000000, 0.9238795325112867385, 1.000000000000000000, 0.9238795325112867385, 1.000000000000000000, 0.9238795325112867385, 1.000000000000000000, 0.9238795325112867385, 1.000000000000000000, 0.9238795325112867385, 1.000000000000000000, 0.9238795325112867385, 1.000000000000000000, 0.9238795325112867385, 1.000000000000000000, 0.9238795325112867385, 1.000000000000000000, 0.9238795325112867385, 1.000000000000000000, 0.9238795325112867385, 1.000000000000000000, 0.9238795325112867385, 1.000000000000000000, 0.9238795325112867385, 1.000000000000000000, 0.9238795325112867385, 1.000000000000000000, 0.9238795325112867385, 1.000000000000000000, 0.9238795325112867385, 1.000000000000000000, 0.9238795325112867385, 1.000000000000000000, 0.9238795325112867385, 1.000000000000000000, 0.9238795325112867385, 1.000000000000000000, 0.9238795325112867385, 1.000000000000000000, 0.9238795325112867385, 1.000000000000000000, 0.9238795325112867385, 1.000000000000000000, 0.9238795325112867385, 1.000000000000000000, 0.9238795325112867385, 1.000000000000000000, 0.9238795325112867385, 1.000000000000000000, 0.9238795325112867385, 1.000000000000000000, 0.9238795325112867385, 1.000000000000000000),
 ( 0.3333333333333333703, 0.3079598441704289313, 0.3333333333333333703, 0.3079598441704289313, 0.3333333333333333703, 0.3079598441704289313, 0.3333333333333333703, 0.3079598441704289313, 0.3333333333333333703, 0.3079598441704289313, 0.3333333333333333703, 0.3079598441704289313, 0.3333333333333333703, 0.3079598441704289313, 0.3333333333333333703, 0.3079598441704289313, 0.3333333333333333703, 0.3079598441704289313, 0.3333333333333333703, 0.3079598441704289313, 0.3333333333333333703, 0.3079598441704289313, 0.3333333333333333703, 0.3079598441704289313, 0.3333333333333333703, 0.3079598441704289313, 0.3333333333333333703, 0.3079598441704289313, 0.3333333333333333703, 0.3079598441704289313, 0.3333333333333333703, 0.3079598441704289313, 0.3333333333333333703, 0.3079598441704289313, 0.3333333333333333703, 0.3079598441704289313, 0.3333333333333333703, 0.3079598441704289313, 0.3333333333333333703, 0.3079598441704289313, 0.3333333333333333703, 0.3079598441704289313, 0.3333333333333333703, 0.3079598441704289313, 0.3333333333333333703, 0.3079598441704289313, 0.3333333333333333703, 0.3079598441704289313, 0.3333333333333333703, 0.3079598441704289313, 0.3333333333333333703, 0.3079598441704289313, 0.3333333333333333703, 0.3079598441704289313, 0.3333333333333333703, 0.3079598441704289313, 0.3333333333333333703, 0.3079598441704289313, 0.3333333333333333703, 0.3079598441704289313, 0.3333333333333333703, 0.3079598441704289313, 0.3333333333333333703, 0.3079598441704289313, 0.3333333333333333703, 0.3079598441704289313, 0.3333333333333333703, 0.3079598441704289313, 0.3333333333333333703, 0.3079598441704289313, 0.3333333333333333703, 0.3079598441704289313, 0.3333333333333333703, 0.3079598441704289313, 0.3333333333333333703, 0.3079598441704289313, 0.3333333333333333703, 0.3079598441704289313, 0.3333333333333333703, 0.3079598441704289313, 0.3333333333333333703, 0.3079598441704289313, 0.3333333333333333703, 0.3079598441704289313, 0.3333333333333333703, 0.3079598441704289313, 0.3333333333333333703, 0.3079598441704289313, 0.3333333333333333703, 0.3079598441704289313, 0.3333333333333333703, 0.3079598441704289313, 0.3333333333333333703, 0.3079598441704289313, 0.3333333333333333703, 0.3079598441704289313, 0.3333333333333333703),
 ( 0.3333333333333333703, 0.3079598441704289313, 0.3333333333333333703, 0.3079598441704289313, 0.3333333333333333703, 0.3079598441704289313, 0.3333333333333333703, 0.3079598441704289313, 0.3333333333333333703, 0.3079598441704289313, 0.3333333333333333703, 0.3079598441704289313, 0.3333333333333333703, 0.3079598441704289313, 0.3333333333333333703, 0.3079598441704289313, 0.3333333333333333703, 0.3079598441704289313, 0.3333333333333333703, 0.3079598441704289313, 0.3333333333333333703, 0.3079598441704289313, 0.3333333333333333703, 0.3079598441704289313, 0.3333333333333333703, 0.3079598441704289313, 0.3333333333333333703, 0.3079598441704289313, 0.3333333333333333703, 0.3079598441704289313, 0.3333333333333333703, 0.3079598441704289313, 0.3333333333333333703, 0.3079598441704289313, 0.3333333333333333703, 0.3079598441704289313, 0.3333333333333333703, 0.3079598441704289313, 0.3333333333333333703, 0.3079598441704289313, 0.3333333333333333703, 0.3079598441704289313, 0.3333333333333333703, 0.3079598441704289313, 0.3333333333333333703, 0.3079598441704289313, 0.3333333333333333703, 0.3079598441704289313, 0.3333333333333333703, 0.3079598441704289313, 0.3333333333333333703, 0.3079598441704289313, 0.3333333333333333703, 0.3079598441704289313, 0.3333333333333333703, 0.3079598441704289313, 0.3333333333333333703, 0.3079598441704289313, 0.3333333333333333703, 0.3079598441704289313, 0.3333333333333333703, 0.3079598441704289313, 0.3333333333333333703, 0.3079598441704289313, 0.3333333333333333703, 0.3079598441704289313, 0.3333333333333333703, 0.3079598441704289313, 0.3333333333333333703, 0.3079598441704289313, 0.3333333333333333703, 0.3079598441704289313, 0.3333333333333333703, 0.3079598441704289313, 0.3333333333333333703, 0.3079598441704289313, 0.3333333333333333703, 0.3079598441704289313, 0.3333333333333333703, 0.3079598441704289313, 0.3333333333333333703, 0.3079598441704289313, 0.3333333333333333703, 0.3079598441704289313, 0.3333333333333333703, 0.3079598441704289313, 0.3333333333333333703, 0.3079598441704289313, 0.3333333333333333703, 0.3079598441704289313, 0.3333333333333333703, 0.3079598441704289313, 0.3333333333333333703, 0.3079598441704289313, 0.3333333333333333703, 0.3079598441704289313, 0.3333333333333333703),
 ( 1.000000000000000000, 0.9238795325112867385, 1.000000000000000000, 0.9238795325112867385, 1.000000000000000000, 0.9238795325112867385, 1.000000000000000000, 0.9238795325112867385, 1.000000000000000000, 0.9238795325112867385, 1.000000000000000000, 0.9238795325112867385, 1.000000000000000000, 0.9238795325112867385, 1.000000000000000000, 0.9238795325112867385, 1.000000000000000000, 0.9238795325112867385, 1.000000000000000000, 0.9238795325112867385, 1.000000000000000000, 0.9238795325112867385, 1.000000000000000000, 0.9238795325112867385, 1.000000000000000000, 0.9238795325112867385, 1.000000000000000000, 0.9238795325112867385, 1.000000000000000000, 0.9238795325112867385, 1.000000000000000000, 0.9238795325112867385, 1.000000000000000000, 0.9238795325112867385, 1.000000000000000000, 0.9238795325112867385, 1.000000000000000000, 0.9238795325112867385, 1.000000000000000000, 0.9238795325112867385, 1.000000000000000000, 0.9238795325112867385, 1.000000000000000000, 0.9238795325112867385, 1.000000000000000000, 0.9238795325112867385, 1.000000000000000000, 0.9238795325112867385, 1.000000000000000000, 0.9238795325112867385, 1.000000000000000000, 0.9238795325112867385, 1.000000000000000000, 0.9238795325112867385, 1.000000000000000000, 0.9238795325112867385, 1.000000000000000000, 0.9238795325112867385, 1.000000000000000000, 0.9238795325112867385, 1.000000000000000000, 0.9238795325112867385, 1.000000000000000000, 0.9238795325112867385, 1.000000000000000000, 0.9238795325112867385, 1.000000000000000000, 0.9238795325112867385, 1.000000000000000000, 0.9238795325112867385, 1.000000000000000000, 0.9238795325112867385, 1.000000000000000000, 0.9238795325112867385, 1.000000000000000000, 0.9238795325112867385, 1.000000000000000000, 0.9238795325112867385, 1.000000000000000000, 0.9238795325112867385, 1.000000000000000000, 0.9238795325112867385, 1.000000000000000000, 0.9238795325112867385, 1.000000000000000000, 0.9238795325112867385, 1.000000000000000000, 0.9238795325112867385, 1.000000000000000000, 0.9238795325112867385, 1.000000000000000000, 0.9238795325112867385, 1.000000000000000000, 0.9238795325112867385, 1.000000000000000000, 0.9238795325112867385, 1.000000000000000000),
 ( 0.3333333333333333703, 0.3079598441704289313, 0.3333333333333333703, 0.3079598441704289313, 0.3333333333333333703, 0.3079598441704289313, 0.3333333333333333703, 0.3079598441704289313, 0.3333333333333333703, 0.3079598441704289313, 0.3333333333333333703, 0.3079598441704289313, 0.3333333333333333703, 0.3079598441704289313, 0.3333333333333333703, 0.3079598441704289313, 0.3333333333333333703, 0.3079598441704289313, 0.3333333333333333703, 0.3079598441704289313, 0.3333333333333333703, 0.3079598441704289313, 0.3333333333333333703, 0.3079598441704289313, 0.3333333333333333703, 0.3079598441704289313, 0.3333333333333333703, 0.3079598441704289313, 0.3333333333333333703, 0.3079598441704289313, 0.3333333333333333703, 0.3079598441704289313, 0.3333333333333333703, 0.3079598441704289313, 0.3333333333333333703, 0.3079598441704289313, 0.3333333333333333703, 0.3079598441704289313, 0.3333333333333333703, 0.3079598441704289313, 0.3333333333333333703, 0.3079598441704289313, 0.3333333333333333703, 0.3079598441704289313, 0.3333333333333333703, 0.3079598441704289313, 0.3333333333333333703, 0.3079598441704289313, 0.3333333333333333703, 0.3079598441704289313, 0.3333333333333333703, 0.3079598441704289313, 0.3333333333333333703, 0.3079598441704289313, 0.3333333333333333703, 0.3079598441704289313, 0.3333333333333333703, 0.3079598441704289313, 0.3333333333333333703, 0.3079598441704289313, 0.3333333333333333703, 0.3079598441704289313, 0.3333333333333333703, 0.3079598441704289313, 0.3333333333333333703, 0.3079598441704289313, 0.3333333333333333703, 0.3079598441704289313, 0.3333333333333333703, 0.3079598441704289313, 0.3333333333333333703, 0.3079598441704289313, 0.3333333333333333703, 0.3079598441704289313, 0.3333333333333333703, 0.3079598441704289313, 0.3333333333333333703, 0.3079598441704289313, 0.3333333333333333703, 0.3079598441704289313, 0.3333333333333333703, 0.3079598441704289313, 0.3333333333333333703, 0.3079598441704289313, 0.3333333333333333703, 0.3079598441704289313, 0.3333333333333333703, 0.3079598441704289313, 0.3333333333333333703, 0.3079598441704289313, 0.3333333333333333703, 0.3079598441704289313, 0.3333333333333333703, 0.3079598441704289313, 0.3333333333333333703, 0.3079598441704289313, 0.3333333333333333703),
 ( 0.3333333333333333703, 0.3079598441704289313, 0.3333333333333333703, 0.3079598441704289313, 0.3333333333333333703, 0.3079598441704289313, 0.3333333333333333703, 0.3079598441704289313, 0.3333333333333333703, 0.3079598441704289313, 0.3333333333333333703, 0.3079598441704289313, 0.3333333333333333703, 0.3079598441704289313, 0.3333333333333333703, 0.3079598441704289313, 0.3333333333333333703, 0.3079598441704289313, 0.3333333333333333703, 0.3079598441704289313, 0.3333333333333333703, 0.3079598441704289313, 0.3333333333333333703, 0.3079598441704289313, 0.3333333333333333703, 0.3079598441704289313, 0.3333333333333333703, 0.3079598441704289313, 0.3333333333333333703, 0.3079598441704289313, 0.3333333333333333703, 0.3079598441704289313, 0.3333333333333333703, 0.3079598441704289313, 0.3333333333333333703, 0.3079598441704289313, 0.3333333333333333703, 0.3079598441704289313, 0.3333333333333333703, 0.3079598441704289313, 0.3333333333333333703, 0.3079598441704289313, 0.3333333333333333703, 0.3079598441704289313, 0.3333333333333333703, 0.3079598441704289313, 0.3333333333333333703, 0.3079598441704289313, 0.3333333333333333703, 0.3079598441704289313, 0.3333333333333333703, 0.3079598441704289313, 0.3333333333333333703, 0.3079598441704289313, 0.3333333333333333703, 0.3079598441704289313, 0.3333333333333333703, 0.3079598441704289313, 0.3333333333333333703, 0.3079598441704289313, 0.3333333333333333703, 0.3079598441704289313, 0.3333333333333333703, 0.3079598441704289313, 0.3333333333333333703, 0.3079598441704289313, 0.3333333333333333703, 0.3079598441704289313, 0.3333333333333333703, 0.3079598441704289313, 0.3333333333333333703, 0.3079598441704289313, 0.3333333333333333703, 0.3079598441704289313, 0.3333333333333333703, 0.3079598441704289313, 0.3333333333333333703, 0.3079598441704289313, 0.3333333333333333703, 0.3079598441704289313, 0.3333333333333333703, 0.3079598441704289313, 0.3333333333333333703, 0.3079598441704289313, 0.3333333333333333703, 0.3079598441704289313, 0.3333333333333333703, 0.3079598441704289313, 0.3333333333333333703, 0.3079598441704289313, 0.3333333333333333703, 0.3079598441704289313, 0.3333333333333333703, 0.3079598441704289313, 0.3333333333333333703, 0.3079598441704289313, 0.3333333333333333703),
 ( 1.000000000000000000, 0.9238795325112867385, 1.000000000000000000, 0.9238795325112867385, 1.000000000000000000, 0.9238795325112867385, 1.000000000000000000, 0.9238795325112867385, 1.000000000000000000, 0.9238795325112867385, 1.000000000000000000, 0.9238795325112867385, 1.000000000000000000, 0.9238795325112867385, 1.000000000000000000, 0.9238795325112867385, 1.000000000000000000, 0.9238795325112867385, 1.000000000000000000, 0.9238795325112867385, 1.000000000000000000, 0.9238795325112867385, 1.000000000000000000, 0.9238795325112867385, 1.000000000000000000, 0.9238795325112867385, 1.000000000000000000, 0.9238795325112867385, 1.000000000000000000, 0.9238795325112867385, 1.000000000000000000, 0.9238795325112867385, 1.000000000000000000, 0.9238795325112867385, 1.000000000000000000, 0.9238795325112867385, 1.000000000000000000, 0.9238795325112867385, 1.000000000000000000, 0.9238795325112867385, 1.000000000000000000, 0.9238795325112867385, 1.000000000000000000, 0.9238795325112867385, 1.000000000000000000, 0.9238795325112867385, 1.000000000000000000, 0.9238795325112867385, 1.000000000000000000, 0.9238795325112867385, 1.000000000000000000, 0.9238795325112867385, 1.000000000000000000, 0.9238795325112867385, 1.000000000000000000, 0.9238795325112867385, 1.000000000000000000, 0.9238795325112867385, 1.000000000000000000, 0.9238795325112867385, 1.000000000000000000, 0.9238795325112867385, 1.000000000000000000, 0.9238795325112867385, 1.000000000000000000, 0.9238795325112867385, 1.000000000000000000, 0.9238795325112867385, 1.000000000000000000, 0.9238795325112867385, 1.000000000000000000, 0.9238795325112867385, 1.000000000000000000, 0.9238795325112867385, 1.000000000000000000, 0.9238795325112867385, 1.000000000000000000, 0.9238795325112867385, 1.000000000000000000, 0.9238795325112867385, 1.000000000000000000, 0.9238795325112867385, 1.000000000000000000, 0.9238795325112867385, 1.000000000000000000, 0.9238795325112867385, 1.000000000000000000, 0.9238795325112867385, 1.000000000000000000, 0.9238795325112867385, 1.000000000000000000, 0.9238795325112867385, 1.000000000000000000, 0.9238795325112867385, 1.000000000000000000, 0.9238795325112867385, 1.000000000000000000) ) ) 
 REPRESENTATION_ITEM ( '' )  SURFACE ( )  );
#3070 = CARTESIAN_POINT ( 'NONE',  ( -9.417894190836991086, 76.54953966738506210, -9.672294700079755003 ) ) ;
#3071 = CARTESIAN_POINT ( 'NONE',  ( -1.541208229742845548, 7.854057316169015479, -18.71369360505681811 ) ) ;
#3072 = FACE_OUTER_BOUND ( 'NONE', #6583, .T. ) ;
#3073 = LINE ( 'NONE', #15081, #16145 ) ;
#3074 = CARTESIAN_POINT ( 'NONE',  ( -4.171729424061791036, 30.53000000000000114, 12.83926296998457239 ) ) ;
#3075 = CARTESIAN_POINT ( 'NONE',  ( 11.76794919243112680, -6.420000000000001705, -3.823638476888993942 ) ) ;
#3076 = CARTESIAN_POINT ( 'NONE',  ( -3.636496289402155746, 36.53000000000000114, 11.19198476289190936 ) ) ;
#3077 = CARTESIAN_POINT ( 'NONE',  ( 1.900613283903584083, 6.237093173894926679, -11.99999999999702993 ) ) ;
#3078 = DIRECTION ( 'NONE',  ( 0.000000000000000000, -0.000000000000000000, 1.000000000000000000 ) ) ;
#3079 = CARTESIAN_POINT ( 'NONE',  ( 13.31658272420281364, 75.35211548525167302, 2.217973532653136459 ) ) ;
#3080 = CIRCLE ( 'NONE', #1386, 12.00000000000000178 ) ;
#3081 = EDGE_CURVE ( 'NONE', #1976, #12212, #1291, .T. ) ;
#3082 = CARTESIAN_POINT ( 'NONE',  ( 10.66011273973178852, 1.083605698617464244E-14, -4.403548868934727523 ) ) ;
#3083 = CARTESIAN_POINT ( 'NONE',  ( 7.272992578804308828, 33.97999999999999687, 10.01041549318726709 ) ) ;
#3084 = CARTESIAN_POINT ( 'NONE',  ( 13.49999999999999822, 80.28000000000000114, 4.386415899144237684 ) ) ;
#3085 = CARTESIAN_POINT ( 'NONE',  ( 10.02787169999155736, 51.77931855093511615, -9.038355711608794252 ) ) ;
#3086 = DIRECTION ( 'NONE',  ( -0.000000000000000000, 1.000000000000000000, -0.000000000000000000 ) ) ;
#3087 = LINE ( 'NONE', #9926, #9516 ) ;
#3088 = CARTESIAN_POINT ( 'NONE',  ( -25.42428528562849266, 0.000000000000000000, -5.441113646577748320 ) ) ;
#3089 = CARTESIAN_POINT ( 'NONE',  ( -4.299010319042174011, 49.33458915034209724, -12.79749347232116996 ) ) ;
#3090 = CARTESIAN_POINT ( 'NONE',  ( 12.57254746066391604, 63.25130592606551261, 4.925209957174280007 ) ) ;
#3091 = CARTESIAN_POINT ( 'NONE',  ( 11.89700905113649476, 42.19366528341078038, 6.391313303333308937 ) ) ;
#3092 = CARTESIAN_POINT ( 'NONE',  ( -18.18516759496687740, 8.007293617507080796, 0.8582236110266343587 ) ) ;
#3093 = CARTESIAN_POINT ( 'NONE',  ( 3.636496289402157078, 24.02999999999999403, -11.19198476289190936 ) ) ;
#3094 = ORIENTED_EDGE ( 'NONE', *, *, #13412, .F. ) ;
#3095 = CARTESIAN_POINT ( 'NONE',  ( -11.76794919243112325, 68.93000000000000682, -2.882316262207890869E-15 ) ) ;
#3096 = CARTESIAN_POINT ( 'NONE',  ( -3.708203932499367195, 3.196025403784437113, -11.41267819554184548 ) ) ;
#3097 = CARTESIAN_POINT ( 'NONE',  ( -8.043339635997654113, -77.00624999999982379, 8.043339635996302306 ) ) ;
#3098 = CARTESIAN_POINT ( 'NONE',  ( -13.50000000000000000, 4.930000000000004157, -3.469446951953614189E-15 ) ) ;
#3099 = VERTEX_POINT ( 'NONE', #15203 ) ;
#3100 = CARTESIAN_POINT ( 'NONE',  ( -2.149914682908597996, 43.25730255030944704, -13.32784165166224888 ) ) ;
#3101 = LINE ( 'NONE', #15201, #5721 ) ;
#3102 = CARTESIAN_POINT ( 'NONE',  ( -13.49999999999999822, 0.07999999999999600486, 4.386415899144235908 ) ) ;
#3103 = EDGE_CURVE ( 'NONE', #2050, #9433, #3959, .T. ) ;
#3104 = CARTESIAN_POINT ( 'NONE',  ( 0.000000000000000000, 3.000000000000000000, 0.000000000000000000 ) ) ;
#3105 = CARTESIAN_POINT ( 'NONE',  ( 12.71198514923275447, 66.26577351268545613, 4.546884237145273566 ) ) ;
#3106 = CARTESIAN_POINT ( 'NONE',  ( 2.933928304667394293, 56.78557572382650420, 13.17766192809576964 ) ) ;
#3107 = CARTESIAN_POINT ( 'NONE',  ( -11.76794919243112325, 62.78000000000000114, -3.823638476888998827 ) ) ;
#3108 = CARTESIAN_POINT ( 'NONE',  ( -7.272992578804310604, 69.38000000000000966, 10.01041549318726709 ) ) ;
#3109 = CARTESIAN_POINT ( 'NONE',  ( -13.48021004250667865, 46.95565286317663833, 0.7426006389843816669 ) ) ;
#3110 = CARTESIAN_POINT ( 'NONE',  ( 5.768599500741140140, 45.97025363302860512, -12.20601842401291570 ) ) ;
#3111 = CARTESIAN_POINT ( 'NONE',  ( -8.891200544363830713E-16, 40.67999999999999261, 13.50000000000000000 ) ) ;
#3112 = CARTESIAN_POINT ( 'NONE',  ( 8.525265987162489623, 30.85325237774112139, -10.46836572103978824 ) ) ;
#3113 = CARTESIAN_POINT ( 'NONE',  ( -8.600387584108450056, 56.34974602370840557, 10.40593404801639643 ) ) ;
#3114 = CARTESIAN_POINT ( 'NONE',  ( -2.124524872238272355, 50.60360011980247208, 13.33178569217110265 ) ) ;
#3115 = CARTESIAN_POINT ( 'NONE',  ( -13.49999999999999822, -9.919999999999999929, 4.386415899144235908 ) ) ;
#3116 = CARTESIAN_POINT ( 'NONE',  ( 11.10072675311360513, 33.14059506802435351, 7.683623606355369340 ) ) ;
#3117 = DIRECTION ( 'NONE',  ( 1.000000000000000000, 0.000000000000000000, 9.821670480311996085E-15 ) ) ;
#3118 = CARTESIAN_POINT ( 'NONE',  ( 0.2341561698673940428, 40.17158518995367444, -13.49825591440075634 ) ) ;
#3119 = CARTESIAN_POINT ( 'NONE',  ( -11.76794919243112325, 24.78000000000000824, -3.823638476888998827 ) ) ;
#3120 = VERTEX_POINT ( 'NONE', #4896 ) ;
#3121 = CARTESIAN_POINT ( 'NONE',  ( -13.47617400855946990, 61.90230964142129011, -0.8017361068469278651 ) ) ;
#3122 = ORIENTED_EDGE ( 'NONE', *, *, #2631, .F. ) ;
#3123 = CARTESIAN_POINT ( 'NONE',  ( -9.520470885617715595, -17.36999999999999744, -6.917026985038136289 ) ) ;
#3124 = CARTESIAN_POINT ( 'NONE',  ( -13.16986379959834252, -30.14374999999995097, -13.16986379960055409 ) ) ;
#3125 = CARTESIAN_POINT ( 'NONE',  ( -12.71700884497776585, 43.76636331146021774, -4.530782870517315430 ) ) ;
#3126 = CARTESIAN_POINT ( 'NONE',  ( -15.58845726811999910, 0.000000000000000000, 10.99999999999985256 ) ) ;
#3127 = CARTESIAN_POINT ( 'NONE',  ( -10.92172942406179104, 38.22999999999999687, 7.935100905948387684 ) ) ;
#3128 = CARTESIAN_POINT ( 'NONE',  ( -8.343458848123582072, 43.38000000000000256, 11.48378591275254124 ) ) ;
#3129 = CARTESIAN_POINT ( 'NONE',  ( 2.207926304393408011E-15, 8.062177826491096155, 17.99999999999999645 ) ) ;
#3130 = CARTESIAN_POINT ( 'NONE',  ( -11.71173941027563359, 67.68051595497325934, -6.714564204021516325 ) ) ;
#3131 = CARTESIAN_POINT ( 'NONE',  ( 7.714727599197340524, -89.52812499999977547, 18.62500000000063949 ) ) ;
#3132 = CARTESIAN_POINT ( 'NONE',  ( 9.353841725489496994, 54.04636460753637550, 9.734530468470028453 ) ) ;
#3133 = EDGE_CURVE ( 'NONE', #6584, #5101, #903, .T. ) ;
#3134 = VERTEX_POINT ( 'NONE', #3735 ) ;
#3135 = CARTESIAN_POINT ( 'NONE',  ( -3.150082944707692345, 64.29333076386686230, -13.12737227364866754 ) ) ;
#3136 = ORIENTED_EDGE ( 'NONE', *, *, #2187, .T. ) ;
#3137 = CARTESIAN_POINT ( 'NONE',  ( 5.329280581304804976, 66.98711426715624384, -12.40357932740702651 ) ) ;
#3138 = CARTESIAN_POINT ( 'NONE',  ( -3.734330915784458860, 34.31427195287466247, -12.97492155557369031 ) ) ;
#3139 = CARTESIAN_POINT ( 'NONE',  ( 4.711679271994909435, -69.72187499999982663, -11.37499999999960387 ) ) ;
#3140 = CARTESIAN_POINT ( 'NONE',  ( 13.07034587478314336, 78.55031594048543298, -3.378768405177414280 ) ) ;
#3141 = CARTESIAN_POINT ( 'NONE',  ( -16.17460542229569498, 8.007813505529846054, 8.351563113033579455 ) ) ;
#3142 = CARTESIAN_POINT ( 'NONE',  ( -4.171729424061787483, 36.32999999999999829, -12.83926296998457417 ) ) ;
#3143 = CARTESIAN_POINT ( 'NONE',  ( 13.17844283097761426, 72.32374584911075033, 3.001318119765830073 ) ) ;
#3144 = CARTESIAN_POINT ( 'NONE',  ( -3.636496289402152637, 27.32999999999999474, -11.19198476289190936 ) ) ;
#3145 = CARTESIAN_POINT ( 'NONE',  ( -10.92172942406179104, 62.23000000000000398, 7.935100905948387684 ) ) ;
#3146 = CARTESIAN_POINT ( 'NONE',  ( -2.598996600649929878, 52.27344996586455750, -13.24758870017709711 ) ) ;
#3147 = CARTESIAN_POINT ( 'NONE',  ( -3.636496289402155746, 39.52999999999999403, 11.19198476289190936 ) ) ;
#3148 = CARTESIAN_POINT ( 'NONE',  ( -13.50000000000000000, 60.92999999999999972, -3.306546357697853733E-15 ) ) ;
#3149 = CIRCLE ( 'NONE', #11349, 5.000000000000000000 ) ;
#3150 = FACE_OUTER_BOUND ( 'NONE', #6063, .T. ) ;
#3151 = CARTESIAN_POINT ( 'NONE',  ( 11.76794919243112325, -3.569999999999996732, 1.734723475976807094E-15 ) ) ;
#3152 = CARTESIAN_POINT ( 'NONE',  ( 8.324673628499295930, 68.99745231419136360, 10.63169888693616372 ) ) ;
#3153 = CARTESIAN_POINT ( 'NONE',  ( -2.736472667029865136, 37.27839283157365458, -13.21980555905066623 ) ) ;
#3154 = CARTESIAN_POINT ( 'NONE',  ( -13.16986379960055409, -100.9062499999997868, 13.16986379959834252 ) ) ;
#3155 = CARTESIAN_POINT ( 'NONE',  ( -11.30478939258968296, 73.65323615164170690, -7.380050224699195915 ) ) ;
#3156 = CARTESIAN_POINT ( 'NONE',  ( -0.5937140765048870561, 76.20134776794657228, -13.49999999999999645 ) ) ;
#3157 = CARTESIAN_POINT ( 'NONE',  ( -13.35138662365028317, 1.798999282680476490E-09, 1.996909364337476678 ) ) ;
#3158 = CARTESIAN_POINT ( 'NONE',  ( 0.000000000000000000, 9.999999999999998224, 0.000000000000000000 ) ) ;
#3159 = DIRECTION ( 'NONE',  ( 0.000000000000000000, 0.000000000000000000, -1.000000000000000000 ) ) ;
#3160 = CARTESIAN_POINT ( 'NONE',  ( 8.343458848123583849, 28.88000000000001322, -11.48378591275253768 ) ) ;
#3161 = CARTESIAN_POINT ( 'NONE',  ( 3.636496289402157078, -8.969999999999998863, -11.19198476289190936 ) ) ;
#3162 = CARTESIAN_POINT ( 'NONE',  ( 3.636496289402154414, 39.82999999999999829, 11.19198476289190936 ) ) ;
#3163 = CARTESIAN_POINT ( 'NONE',  ( -4.171729424061787483, -13.66999999999999460, -12.83926296998457417 ) ) ;
#3164 = AXIS2_PLACEMENT_3D ( 'NONE', #11409, #3521, #1926 ) ;
#3165 = CARTESIAN_POINT ( 'NONE',  ( -11.20853034038327856, 32.21278346977177165, 7.524684492930465041 ) ) ;
#3166 = CARTESIAN_POINT ( 'NONE',  ( 1.204043358265280084, 74.72328260670963118, 13.44640036567524355 ) ) ;
#3167 = CARTESIAN_POINT ( 'NONE',  ( 18.55549153077629398, 8.384379708534148161E-15, -1.770424328178711759 ) ) ;
#3168 = PRODUCT_DEFINITION ( 'UNKNOWN', '', #8215, #7745 ) ;
#3169 = CARTESIAN_POINT ( 'NONE',  ( -11.76794919243112325, 32.92999999999999972, -2.882316262207890869E-15 ) ) ;
#3170 = CARTESIAN_POINT ( 'NONE',  ( -1.731132465502642548, 58.24222653993336252, -13.39023422218494197 ) ) ;
#3171 =( BOUNDED_CURVE ( )  B_SPLINE_CURVE ( 2, ( #10598, #948, #12895, #3695, #15960, #2348, #8850, #14204, #10679, #6621, #245, #14980, #2784 ),
 .UNSPECIFIED., .F., .F. ) 
 B_SPLINE_CURVE_WITH_KNOTS ( ( 3, 2, 2, 2, 2, 2, 3 ),
 ( 0.6250000000000000000, 0.6277777777777777679, 0.6333333333333333037, 0.6388888888888888395, 0.6444444444444444864, 0.6500000000000000222, 0.6527777777777777901 ),
 .UNSPECIFIED. ) 
 CURVE ( )  GEOMETRIC_REPRESENTATION_ITEM ( )  RATIONAL_B_SPLINE_CURVE ( ( 0.9755282581475768211, 0.9755282581475768211, 1.000000000000000000, 0.9510565162951535312, 1.000000000000000000, 0.9510565162951535312, 1.000000000000000000, 0.9510565162951535312, 1.000000000000000000, 0.9510565162951535312, 1.000000000000000000, 0.9755282581475768211, 0.9755282581475768211 ) ) 
 REPRESENTATION_ITEM ( '' )  );
#3172 = CARTESIAN_POINT ( 'NONE',  ( -4.334019030006316164, 38.52414229972498561, 12.78541219897794790 ) ) ;
#3173 = AXIS2_PLACEMENT_3D ( 'NONE', #7291, #7642, #10209 ) ;
#3174 = CARTESIAN_POINT ( 'NONE',  ( 0.1389302926457151033, 37.17500468106219103, -13.49929213118588223 ) ) ;
#3175 = EDGE_CURVE ( 'NONE', #6231, #11897, #12829, .T. ) ;
#3176 = CARTESIAN_POINT ( 'NONE',  ( -10.92172942406179104, 70.23000000000000398, 7.935100905948387684 ) ) ;
#3177 = ADVANCED_FACE ( 'NONE', ( #716 ), #14221, .F. ) ;
#3178 = CARTESIAN_POINT ( 'NONE',  ( -9.999999999999776179, 0.000000000000000000, -17.32050807568890605 ) ) ;
#3179 = CARTESIAN_POINT ( 'NONE',  ( 2.636466003486186427, 62.77480020505506531, 13.24005480980223659 ) ) ;
#3180 = CARTESIAN_POINT ( 'NONE',  ( 7.801031699874362957, 41.97399651719818792, 11.02225216533711283 ) ) ;
#3181 = CARTESIAN_POINT ( 'NONE',  ( 10.80204579108763774, 48.73690422266599853, -8.097748324130661146 ) ) ;
#3182 = CARTESIAN_POINT ( 'NONE',  ( 11.76794919243112680, 23.58000000000001961, -3.823638476888993942 ) ) ;
#3183 = ORIENTED_EDGE ( 'NONE', *, *, #10372, .T. ) ;
#3184 = CARTESIAN_POINT ( 'NONE',  ( -7.576616670048093940E-16, 69.68000000000000682, 12.37355403259654807 ) ) ;
#3185 = CARTESIAN_POINT ( 'NONE',  ( -4.711679271994916540, -4.196874999999971934, 11.37499999999960565 ) ) ;
#3186 = CARTESIAN_POINT ( 'NONE',  ( 11.37500000000000000, -83.24999999999980105, 9.531744055041752924E-13 ) ) ;
#3187 = CARTESIAN_POINT ( 'NONE',  ( -8.343458848123576743, 10.48000000000000753, -11.48378591275254301 ) ) ;
#3188 = ORIENTED_EDGE ( 'NONE', *, *, #7234, .F. ) ;
#3189 = CARTESIAN_POINT ( 'NONE',  ( -1.644898173497524319, 43.23913777945310954, -13.40128083404708903 ) ) ;
#3190 = CARTESIAN_POINT ( 'NONE',  ( -10.16154112307833302, 80.93000000000002103, -6.935345943057503959 ) ) ;
#3191 = CARTESIAN_POINT ( 'NONE',  ( 8.343458848123583849, 1.879999999999997451, -11.48378591275253768 ) ) ;
#3192 = DIRECTION ( 'NONE',  ( 0.000000000000000000, 0.000000000000000000, 1.000000000000000000 ) ) ;
#3193 = CARTESIAN_POINT ( 'NONE',  ( 18.62500000000000000, -16.64999999999995950, 1.560692158462880521E-12 ) ) ;
#3194 = CARTESIAN_POINT ( 'NONE',  ( 6.054972155430796477, 65.90111290053462767, 12.06729893293001510 ) ) ;
#3195 = CARTESIAN_POINT ( 'NONE',  ( 10.03637343360090561, 57.08084545600886628, 9.039336760165353368 ) ) ;
#3196 = CARTESIAN_POINT ( 'NONE',  ( 2.272985001014427788E-15, 62.17999999999999972, -12.37355403259654985 ) ) ;
#3197 = CARTESIAN_POINT ( 'NONE',  ( -13.50000000000000000, 33.92999999999999972, -3.306546357697853733E-15 ) ) ;
#3198 = CARTESIAN_POINT ( 'NONE',  ( -11.76794919243112325, 69.08000000000001251, 3.823638476888994386 ) ) ;
#3199 = CARTESIAN_POINT ( 'NONE',  ( -11.32567959555823833, 46.65459798133181124, -7.347039100656743038 ) ) ;
#3200 = CARTESIAN_POINT ( 'NONE',  ( 9.958918772552300069, 45.78319215442776624, -9.126329330056044853 ) ) ;
#3201 = CARTESIAN_POINT ( 'NONE',  ( 6.668229702898669231, 69.93442387800766369, -11.75383367542387525 ) ) ;
#3202 = MANIFOLD_SOLID_BREP ( 'Cut-Extrude2', #5220 ) ;
#3203 = CARTESIAN_POINT ( 'NONE',  ( -12.50000000000000000, -18.00000000000000355, -2.204364238465235822E-15 ) ) ;
#3204 = CARTESIAN_POINT ( 'NONE',  ( 0.1136162170211922895, 31.17591480126643688, -13.49958623107663236 ) ) ;
#3205 = CARTESIAN_POINT ( 'NONE',  ( -13.23950142262943785, 56.02442396258347657, 2.673273018928831846 ) ) ;
#3206 = EDGE_CURVE ( 'NONE', #9217, #1172, #11808, .T. ) ;
#3207 = CARTESIAN_POINT ( 'NONE',  ( -0.8894439718356197400, 50.64828125085173838, 13.47800680310904475 ) ) ;
#3208 = CARTESIAN_POINT ( 'NONE',  ( 5.597103228875909053, 32.88291356958394829, 12.29308424054071658 ) ) ;
#3209 = CARTESIAN_POINT ( 'NONE',  ( 1.133320036021603139, 9.999999999999996447, 13.00525967219381762 ) ) ;
#3210 = CARTESIAN_POINT ( 'NONE',  ( 9.391517042431177131, 39.81199946441067539, -9.706920749962888451 ) ) ;
#3211 = VERTEX_POINT ( 'NONE', #2041 ) ;
#3212 = CARTESIAN_POINT ( 'NONE',  ( -13.49217480359717491, 61.94797010018912431, 0.5234354021173442950 ) ) ;
#3213 = ORIENTED_EDGE ( 'NONE', *, *, #13130, .F. ) ;
#3214 = CARTESIAN_POINT ( 'NONE',  ( 13.50000000000000355, 33.58000000000000540, -4.386415899144233244 ) ) ;
#3215 = CARTESIAN_POINT ( 'NONE',  ( -18.62500000000000000, -48.87499999999990052, -1.562973063126292757E-12 ) ) ;
#3216 = CARTESIAN_POINT ( 'NONE',  ( 2.445080149700053643E-15, 66.18000000000000682, -13.50000000000000000 ) ) ;
#3217 = CARTESIAN_POINT ( 'NONE',  ( -10.92172942406178926, 31.62999999999999901, -7.935100905948389460 ) ) ;
#3218 = CARTESIAN_POINT ( 'NONE',  ( -8.343458848123576743, 39.48000000000000398, -11.48378591275254301 ) ) ;
#3219 = CARTESIAN_POINT ( 'NONE',  ( -6.307303722844142868, 46.41121506314294010, -11.93599373864252478 ) ) ;
#3220 = CARTESIAN_POINT ( 'NONE',  ( -2.609388387809556953, 67.27396147325951858, -13.24715127702997997 ) ) ;
#3221 = CARTESIAN_POINT ( 'NONE',  ( -11.37499999999960743, -0.03437499999998146899, -4.711679271994912099 ) ) ;
#3222 = EDGE_CURVE ( 'NONE', #8820, #967, #8099, .T. ) ;
#3223 = CARTESIAN_POINT ( 'NONE',  ( 10.68409364263760963, 54.11638383922162632, 8.252282988383353057 ) ) ;
#3224 = CARTESIAN_POINT ( 'NONE',  ( 3.636496289402157078, 15.03000000000001535, -11.19198476289190936 ) ) ;
#3225 = ORIENTED_EDGE ( 'NONE', *, *, #14449, .F. ) ;
#3226 = CARTESIAN_POINT ( 'NONE',  ( -3.283445202252278428, 64.29804246037801363, -13.09461853665598774 ) ) ;
#3227 = ORIENTED_EDGE ( 'NONE', *, *, #237, .T. ) ;
#3228 = CARTESIAN_POINT ( 'NONE',  ( -8.891200544363830713E-16, 8.679999999999999716, 13.49999999999999822 ) ) ;
#3229 = CARTESIAN_POINT ( 'NONE',  ( -8.075662332356120743, 34.48627614415578080, -10.81823397106624363 ) ) ;
#3230 = CARTESIAN_POINT ( 'NONE',  ( -11.37500000000000000, -74.92499999999982663, -9.545674412382054647E-13 ) ) ;
#3231 = CARTESIAN_POINT ( 'NONE',  ( 4.135038185100354369, 77.82866846073966371, 12.85155843290215394 ) ) ;
#3232 = CARTESIAN_POINT ( 'NONE',  ( 4.171729424061791924, 48.02999999999999403, -12.83926296998457239 ) ) ;
#3233 = DIRECTION ( 'NONE',  ( 0.000000000000000000, 1.000000000000000000, 0.000000000000000000 ) ) ;
#3234 = CARTESIAN_POINT ( 'NONE',  ( -11.00000000000012612, 0.000000000000000000, 15.58845726811980725 ) ) ;
#3235 = CARTESIAN_POINT ( 'NONE',  ( 11.47066830352881439, 72.16402218860807238, 7.118558593351406394 ) ) ;
#3236 = CARTESIAN_POINT ( 'NONE',  ( 7.272992578804311492, 32.88000000000000256, -10.01041549318726709 ) ) ;
#3237 = CARTESIAN_POINT ( 'NONE',  ( -13.49999999999999822, 61.77999999999998693, -4.386415899144240349 ) ) ;
#3238 = CARTESIAN_POINT ( 'NONE',  ( -8.798805876808101445, 52.51956008151021393, -10.23871025406966062 ) ) ;
#3239 = CARTESIAN_POINT ( 'NONE',  ( 8.343458848123578520, 61.97999999999998977, 11.48378591275254124 ) ) ;
#3240 = FACE_OUTER_BOUND ( 'NONE', #5359, .T. ) ;
#3241 = CARTESIAN_POINT ( 'NONE',  ( -11.76794919243112325, -2.069999999999995399, -2.602085213965210642E-15 ) ) ;
#3242 = CARTESIAN_POINT ( 'NONE',  ( 10.88591283206684857, 69.12792091989102516, 7.984178984618108821 ) ) ;
#3243 = CARTESIAN_POINT ( 'NONE',  ( -13.16986379959834252, -6.243749999999985256, -13.16986379960055054 ) ) ;
#3244 = CARTESIAN_POINT ( 'NONE',  ( 8.343458848123580296, 70.98000000000000398, 11.48378591275253768 ) ) ;
#3245 = CARTESIAN_POINT ( 'NONE',  ( -1.564113515457998370E-12, -53.03749999999988773, 18.62500000000000000 ) ) ;
#3246 = CARTESIAN_POINT ( 'NONE',  ( -10.59251559326346559, 73.61123193496310080, -8.369515937429383712 ) ) ;
#3247 = DIRECTION ( 'NONE',  ( 0.000000000000000000, 0.000000000000000000, 1.000000000000000000 ) ) ;
#3248 = CARTESIAN_POINT ( 'NONE',  ( -4.702552466601850334, 79.34928690549976693, -12.65703117179169546 ) ) ;
#3249 = CARTESIAN_POINT ( 'NONE',  ( -17.42428528562871293, 0.000000000000000000, 19.29752010712834220 ) ) ;
#3250 = CARTESIAN_POINT ( 'NONE',  ( 13.50000000000000000, 31.43000000000001393, 1.734723475976807094E-15 ) ) ;
#3251 = CARTESIAN_POINT ( 'NONE',  ( 9.520470885617717371, -6.269999999999997797, -6.917026985038131848 ) ) ;
#3252 = CARTESIAN_POINT ( 'NONE',  ( -7.272992578804310604, 39.37999999999999545, 10.01041549318726886 ) ) ;
#3253 = AXIS2_PLACEMENT_3D ( 'NONE', #7880, #1398, #2540 ) ;
#3254 = UNCERTAINTY_MEASURE_WITH_UNIT (LENGTH_MEASURE( 1.000000000000000082E-05 ), #14174, 'distance_accuracy_value', 'NONE');
#3255 = CARTESIAN_POINT ( 'NONE',  ( -4.171729424061791036, -15.46999999999999709, 12.83926296998457239 ) ) ;
#3256 = APPLICATION_CONTEXT ( 'automotive_design' ) ;
#3257 = CARTESIAN_POINT ( 'NONE',  ( -1.735113556039163285, 32.61758944806980764, 13.38823632957157983 ) ) ;
#3258 = CARTESIAN_POINT ( 'NONE',  ( 3.688403295120684433, 74.81262137495812681, 12.98636652492995580 ) ) ;
#3259 = CARTESIAN_POINT ( 'NONE',  ( 8.343458848123580296, 2.979999999999998650, 11.48378591275253768 ) ) ;
#3260 = MANIFOLD_SOLID_BREP ( 'Combine1', #4371 ) ;
#3261 = EDGE_CURVE ( 'NONE', #8284, #11444, #7607, .T. ) ;
#3262 =( NAMED_UNIT ( * ) PLANE_ANGLE_UNIT ( ) SI_UNIT ( $, .RADIAN. ) );
#3263 = CARTESIAN_POINT ( 'NONE',  ( 8.343458848123583849, 83.87999999999998124, -11.48378591275253768 ) ) ;
#3264 = CARTESIAN_POINT ( 'NONE',  ( 9.810655436414416286, 51.79065996878712497, -9.275473329678410650 ) ) ;
#3265 =( GEOMETRIC_REPRESENTATION_CONTEXT ( 3 ) GLOBAL_UNCERTAINTY_ASSIGNED_CONTEXT ( ( #15266 ) ) GLOBAL_UNIT_ASSIGNED_CONTEXT ( ( #8539, #13889, #14068 ) ) REPRESENTATION_CONTEXT ( 'NONE', 'WORKASPACE' ) );
#3266 = CARTESIAN_POINT ( 'NONE',  ( -6.694392717615978761, 38.43308941745874563, 11.72613373514175095 ) ) ;
#3267 = DIRECTION ( 'NONE',  ( 0.000000000000000000, 1.000000000000000000, 0.000000000000000000 ) ) ;
#3268 = FACE_OUTER_BOUND ( 'NONE', #4170, .T. ) ;
#3269 = DIRECTION ( 'NONE',  ( 0.000000000000000000, -1.000000000000000000, 0.000000000000000000 ) ) ;
#3270 = CARTESIAN_POINT ( 'NONE',  ( 9.614817975872671951, 63.05940465635595160, 9.476564584252601620 ) ) ;
#3271 = CARTESIAN_POINT ( 'NONE',  ( 8.000000000000023093, 0.000000000000000000, -17.32050807568876394 ) ) ;
#3272 = CARTESIAN_POINT ( 'NONE',  ( 13.20987146810338686, 48.52847080726490248, -2.784488331728600663 ) ) ;
#3273 = CARTESIAN_POINT ( 'NONE',  ( 9.520470885617717371, 17.72999999999999687, -6.917026985038131848 ) ) ;
#3274 = VERTEX_POINT ( 'NONE', #474 ) ;
#3275 = CARTESIAN_POINT ( 'NONE',  ( 3.636496289402157078, 65.03000000000000114, -11.19198476289190936 ) ) ;
#3276 = CARTESIAN_POINT ( 'NONE',  ( 9.538709233711902776E-13, -13.56249999999995026, -11.37500000000000178 ) ) ;
#3277 = CARTESIAN_POINT ( 'NONE',  ( -11.37499999999960387, -23.93437499999994245, -4.711679271994911211 ) ) ;
#3278 = CARTESIAN_POINT ( 'NONE',  ( -13.49999999999999822, 4.780000000000001137, -4.386415899144240349 ) ) ;
#3279 = CARTESIAN_POINT ( 'NONE',  ( 7.272992578804311492, 32.88000000000000256, -10.01041549318726709 ) ) ;
#3280 = CARTESIAN_POINT ( 'NONE',  ( -9.999999999999776179, 0.000000000000000000, -15.32050807568890605 ) ) ;
#3281 = AXIS2_PLACEMENT_3D ( 'NONE', #1187, #1269, #10400 ) ;
#3282 = CARTESIAN_POINT ( 'NONE',  ( 4.171729424061789260, 6.830000000000002736, 12.83926296998457239 ) ) ;
#3283 = CARTESIAN_POINT ( 'NONE',  ( -18.62500000000000000, -24.97499999999994102, -1.562973063126292555E-12 ) ) ;
#3284 = CARTESIAN_POINT ( 'NONE',  ( 8.411964441243910073, 66.00153322346682216, 10.55915802395268344 ) ) ;
#3285 = LINE ( 'NONE', #14231, #303 ) ;
#3286 = EDGE_CURVE ( 'NONE', #14568, #15151, #11437, .T. ) ;
#3287 =( BOUNDED_CURVE ( )  B_SPLINE_CURVE ( 2, ( #4423, #3077, #1837, #8504, #13853, #1756, #7252, #16691, #4598, #2006, #12812, #11745, #3603 ),
 .UNSPECIFIED., .F., .F. ) 
 B_SPLINE_CURVE_WITH_KNOTS ( ( 3, 2, 2, 2, 2, 2, 3 ),
 ( 0.09225345574959326056, 0.09600779387844439461, 0.1035164701361835637, 0.1110251463939227468, 0.1185338226516619159, 0.1260424989094010850, 0.1297968370382597270 ),
 .UNSPECIFIED. ) 
 CURVE ( )  GEOMETRIC_REPRESENTATION_ITEM ( )  RATIONAL_B_SPLINE_CURVE ( ( 0.9755282581475768211, 0.9755282581476976134, 1.000000000000000000, 0.9510565162951535312, 1.000000000000000000, 0.9510565162951535312, 1.000000000000000000, 0.9510565162951535312, 1.000000000000000000, 0.9510565162951535312, 1.000000000000000000, 0.9755282581476480974, 0.9755282581475767101 ) ) 
 REPRESENTATION_ITEM ( '' )  );
#3288 = CARTESIAN_POINT ( 'NONE',  ( 11.76794919243112680, 49.57999999999999119, -3.823638476888993942 ) ) ;
#3289 = CARTESIAN_POINT ( 'NONE',  ( -7.576616670048093940E-16, 57.67999999999999261, 12.37355403259654985 ) ) ;
#3290 = CARTESIAN_POINT ( 'NONE',  ( -10.30583073249865045, 46.59490174438735721, -8.728845011251372910 ) ) ;
#3291 = CARTESIAN_POINT ( 'NONE',  ( 7.506318827951740325, 45.89879490785331484, -11.22085109350133614 ) ) ;
#3292 = CARTESIAN_POINT ( 'NONE',  ( 5.745986813403028748, 69.97110941641926729, -12.21637056639575292 ) ) ;
#3293 = B_SPLINE_CURVE_WITH_KNOTS ( 'NONE', 3,
 ( #305, #8455, #129, #4283 ),
 .UNSPECIFIED., .F., .F.,
 ( 4, 4 ),
 ( 2.383248697827832346E-07, 0.007646667935218598965 ),
 .UNSPECIFIED. ) ;
#3294 = SURFACE_SIDE_STYLE ('',( #5793 ) ) ;
#3295 = CARTESIAN_POINT ( 'NONE',  ( 0.2317842287749069252, 31.17166591792411978, -13.49801495282379094 ) ) ;
#3296 = CARTESIAN_POINT ( 'NONE',  ( -13.49470243760989696, 55.91483651601082983, -0.4366705576521556220 ) ) ;
#3297 = VECTOR ( 'NONE', #6335, 1000.000000000000000 ) ;
#3298 = CARTESIAN_POINT ( 'NONE',  ( -11.00000000000012612, 0.000000000000000000, 15.58845726811980725 ) ) ;
#3299 = CARTESIAN_POINT ( 'NONE',  ( 0.5562443415044789896, 32.70003642497442797, 13.49174744467049258 ) ) ;
#3300 = CARTESIAN_POINT ( 'NONE',  ( 2.804204357426235195, 43.07917734367891427, -13.20558232696900980 ) ) ;
#3301 = CARTESIAN_POINT ( 'NONE',  ( 6.372342379802677925, 39.94615721271951969, -11.90962055736550518 ) ) ;
#3302 = EDGE_LOOP ( 'NONE', ( #7735, #9347, #14761, #9523, #1552, #7644 ) ) ;
#3303 = CARTESIAN_POINT ( 'NONE',  ( -10.74856790587859479, 62.24021944068277179, 8.173410186847442915 ) ) ;
#3304 = ORIENTED_EDGE ( 'NONE', *, *, #12057, .F. ) ;
#3305 = CARTESIAN_POINT ( 'NONE',  ( 11.76794919243112325, -18.72000000000000952, 3.823638476888996163 ) ) ;
#3306 = CARTESIAN_POINT ( 'NONE',  ( -13.16986379960055409, -100.9062499999997868, 13.16986379959834252 ) ) ;
#3307 = SURFACE_SIDE_STYLE ('',( #13811 ) ) ;
#3308 = CARTESIAN_POINT ( 'NONE',  ( 11.19043610557870494, 48.14612993255676088, 7.554903771323779438 ) ) ;
#3309 = CARTESIAN_POINT ( 'NONE',  ( 2.450181162087849529, 58.09190187880095380, -13.27579793785504059 ) ) ;
#3310 = CARTESIAN_POINT ( 'NONE',  ( -13.49999999999999822, 32.07999999999999829, 4.386415899144235908 ) ) ;
#3311 = CARTESIAN_POINT ( 'NONE',  ( 11.33202052101486146, -2.258074356960819520E-15, 6.793706961618169338 ) ) ;
#3312 = EDGE_CURVE ( 'NONE', #15652, #7559, #10626, .T. ) ;
#3313 = CARTESIAN_POINT ( 'NONE',  ( -12.50000000000000000, -18.00000000000000355, -2.204364238465235822E-15 ) ) ;
#3314 = CARTESIAN_POINT ( 'NONE',  ( 0.000000000000000000, 75.00000000000000000, 0.000000000000000000 ) ) ;
#3315 = CARTESIAN_POINT ( 'NONE',  ( 11.37499999999960565, -25.00937499999992397, 4.711679271994918317 ) ) ;
#3316 = CARTESIAN_POINT ( 'NONE',  ( 5.022062556576507575, 53.86124677859262277, 12.53116408511900381 ) ) ;
#3317 = ORIENTED_EDGE ( 'NONE', *, *, #12615, .T. ) ;
#3318 = DIRECTION ( 'NONE',  ( -0.000000000000000000, -1.000000000000000000, -0.000000000000000000 ) ) ;
#3319 = EDGE_LOOP ( 'NONE', ( #3477, #8212, #14391, #16991 ) ) ;
#3320 = CARTESIAN_POINT ( 'NONE',  ( 5.639642118617593347, 66.97529727505714447, -12.26620933673328473 ) ) ;
#3321 = CARTESIAN_POINT ( 'NONE',  ( -4.034686368860703531, 34.32507233461874563, -12.88341026651710486 ) ) ;
#3322 = B_SPLINE_CURVE_WITH_KNOTS ( 'NONE', 3,
 ( #6401, #4892, #9149, #13018 ),
 .UNSPECIFIED., .F., .F.,
 ( 4, 4 ),
 ( 2.383248697861188768E-07, 0.007646667935218605036 ),
 .UNSPECIFIED. ) ;
#3323 = CARTESIAN_POINT ( 'NONE',  ( 9.538709233711902776E-13, -28.06249999999995381, -11.37499999999999645 ) ) ;
#3324 = CARTESIAN_POINT ( 'NONE',  ( 4.285061171620013099, 77.83408588564444130, 12.80199298906653382 ) ) ;
#3325 = CARTESIAN_POINT ( 'NONE',  ( -8.891200544363830713E-16, 46.67999999999999972, 13.50000000000000000 ) ) ;
#3326 = CARTESIAN_POINT ( 'NONE',  ( 17.32050807568873552, 7.773118517290098062, 8.000000000000083489 ) ) ;
#3327 = CARTESIAN_POINT ( 'NONE',  ( -13.49999999999999822, 6.080000000000002736, 4.386415899144235020 ) ) ;
#3328 = CARTESIAN_POINT ( 'NONE',  ( 12.93105386136839563, 72.56893679360238991, -3.878076313447386791 ) ) ;
#3329 = CARTESIAN_POINT ( 'NONE',  ( 7.586958922275961470, 66.89532775841007606, -11.16783085649728591 ) ) ;
#3330 = CARTESIAN_POINT ( 'NONE',  ( -3.636496289402152637, 33.32999999999999829, -11.19198476289190936 ) ) ;
#3331 = CARTESIAN_POINT ( 'NONE',  ( -8.691771469529815392E-16, 65.68000000000000682, 14.19474002721660355 ) ) ;
#3332 = CARTESIAN_POINT ( 'NONE',  ( -10.59755759974650680, 52.60935872665269386, -8.433183405451526227 ) ) ;
#3333 = ADVANCED_FACE ( 'NONE', ( #811 ), #1161, .T. ) ;
#3334 = CARTESIAN_POINT ( 'NONE',  ( 11.76794919243112680, 34.57999999999999829, -3.823638476888993942 ) ) ;
#3335 = CARTESIAN_POINT ( 'NONE',  ( -7.272992578804307939, -14.51999999999999957, -10.01041549318726886 ) ) ;
#3336 = CARTESIAN_POINT ( 'NONE',  ( -13.49999999999999822, 55.08000000000000540, 4.386415899144235908 ) ) ;
#3337 = LINE ( 'NONE', #11478, #7034 ) ;
#3338 = CARTESIAN_POINT ( 'NONE',  ( 7.272992578804311492, -0.1199999999999976641, -10.01041549318726709 ) ) ;
#3339 = CARTESIAN_POINT ( 'NONE',  ( -4.376496056507735766, 68.52259899468778315, 12.77091595960407489 ) ) ;
#3340 = CARTESIAN_POINT ( 'NONE',  ( 7.714727599197338748, -30.17812499999993747, 18.62500000000063949 ) ) ;
#3341 = CARTESIAN_POINT ( 'NONE',  ( -4.206197538246631673, 6.548267719634617734, 23.28534784291397131 ) ) ;
#3342 = AXIS2_PLACEMENT_3D ( 'NONE', #12452, #15164, #8489 ) ;
#3343 = CARTESIAN_POINT ( 'NONE',  ( 1.561832610794586538E-12, -4.162499999999989875, -18.62500000000000000 ) ) ;
#3344 = CARTESIAN_POINT ( 'NONE',  ( -13.37666621905920650, 73.99562545368686983, 1.878105658975215420 ) ) ;
#3345 = CARTESIAN_POINT ( 'NONE',  ( 5.441113646577480978, 5.918584287042170544, -25.42428528562854595 ) ) ;
#3346 = CARTESIAN_POINT ( 'NONE',  ( -11.00000000000012612, 7.773118517290097174, 15.58845726811980725 ) ) ;
#3347 = DIRECTION ( 'NONE',  ( 0.000000000000000000, 0.000000000000000000, -1.000000000000000000 ) ) ;
#3348 = CARTESIAN_POINT ( 'NONE',  ( 9.520470885617715595, 34.13000000000000256, 6.917026985038134512 ) ) ;
#3349 = DIRECTION ( 'NONE',  ( 0.000000000000000000, 0.000000000000000000, -1.000000000000000000 ) ) ;
#3350 = CARTESIAN_POINT ( 'NONE',  ( -1.471122160089594955, 32.62715143919767513, 13.41980678565153795 ) ) ;
#3351 = DIRECTION ( 'NONE',  ( -0.000000000000000000, 1.000000000000000000, -0.000000000000000000 ) ) ;
#3352 = CARTESIAN_POINT ( 'NONE',  ( 2.138189944381259977, 61.75688142232026934, 13.49999999999999289 ) ) ;
#3353 = AXIS2_PLACEMENT_3D ( 'NONE', #9165, #13035, #11538 ) ;
#3354 = CARTESIAN_POINT ( 'NONE',  ( -13.49999999999999822, 79.07999999999999829, 4.386415899144235908 ) ) ;
#3355 = CARTESIAN_POINT ( 'NONE',  ( 12.48859630623820038, 51.61660746006936762, -5.128397564142412435 ) ) ;
#3356 = CARTESIAN_POINT ( 'NONE',  ( -7.028416087530689360, 38.41914928954428632, 11.52616306344620689 ) ) ;
#3357 = DIRECTION ( 'NONE',  ( 0.000000000000000000, 1.000000000000000000, 0.000000000000000000 ) ) ;
#3358 = CARTESIAN_POINT ( 'NONE',  ( 4.711679271993006068, -63.47812499999984226, 11.37500000000039257 ) ) ;
#3359 = CARTESIAN_POINT ( 'NONE',  ( 1.732050807568740858, 0.000000000000000000, 19.00000000000000355 ) ) ;
#3360 = FACE_OUTER_BOUND ( 'NONE', #8104, .T. ) ;
#3361 = CARTESIAN_POINT ( 'NONE',  ( 0.07515814835109146941, 62.68270335294189266, 13.49999999999987033 ) ) ;
#3362 = CARTESIAN_POINT ( 'NONE',  ( 3.518843866200051185, 41.80622085848303016, 13.03652279665081615 ) ) ;
#3363 = CARTESIAN_POINT ( 'NONE',  ( 10.73149705005626409, 48.74093281793692256, -8.190661608126919901 ) ) ;
#3364 = AXIS2_PLACEMENT_3D ( 'NONE', #15668, #2404, #3576 ) ;
#3365 = CARTESIAN_POINT ( 'NONE',  ( 2.279995255611139653E-15, 18.18000000000001393, -12.37355403259654985 ) ) ;
#3366 = EDGE_CURVE ( 'NONE', #8302, #12894, #4887, .T. ) ;
#3367 = ORIENTED_EDGE ( 'NONE', *, *, #4951, .T. ) ;
#3368 = CARTESIAN_POINT ( 'NONE',  ( -3.636496289402155746, 63.53000000000000114, 11.19198476289190936 ) ) ;
#3369 = CARTESIAN_POINT ( 'NONE',  ( 18.62499999999935341, -74.95937499999980957, 7.714727599200469577 ) ) ;
#3370 = CARTESIAN_POINT ( 'NONE',  ( -9.552639591052204498E-13, -62.43749999999985079, 11.37500000000000000 ) ) ;
#3371 = CARTESIAN_POINT ( 'NONE',  ( -10.92172942406179104, -0.7699999999999929123, 7.935100905948385908 ) ) ;
#3372 = DIRECTION ( 'NONE',  ( -0.000000000000000000, -1.000000000000000000, -0.000000000000000000 ) ) ;
#3373 = CARTESIAN_POINT ( 'NONE',  ( -7.321446643551189126, 80.93000000000003524, -10.20755442052239026 ) ) ;
#3374 = CARTESIAN_POINT ( 'NONE',  ( 18.62500000000064304, -67.64062499999984368, -7.714727599197334307 ) ) ;
#3375 = CARTESIAN_POINT ( 'NONE',  ( 11.72063973829996009, 66.18111146641619769, 6.700015991577908281 ) ) ;
#3376 = CARTESIAN_POINT ( 'NONE',  ( -4.206197538246465584, 6.548267719634618622, -23.28534784291399973 ) ) ;
#3377 = CARTESIAN_POINT ( 'NONE',  ( -7.272992578804310604, 51.37999999999998835, 10.01041549318726709 ) ) ;
#3378 = CARTESIAN_POINT ( 'NONE',  ( -8.343458848123576743, 33.47999999999999687, -11.48378591275254301 ) ) ;
#3379 = CARTESIAN_POINT ( 'NONE',  ( -13.32459686664603282, 46.85386381616618223, -2.169380165940829386 ) ) ;
#3380 = AXIS2_PLACEMENT_3D ( 'NONE', #4287, #5629, #12153 ) ;
#3381 = CARTESIAN_POINT ( 'NONE',  ( 9.153033843582718987, 45.82346993534611812, -9.923304509235496340 ) ) ;
#3382 = CARTESIAN_POINT ( 'NONE',  ( 9.813981802417188760, 69.79049870256335453, -9.272224570126397225 ) ) ;
#3383 = CARTESIAN_POINT ( 'NONE',  ( -1.900613283894436512, 7.737093173895296161, 12.00000000000000178 ) ) ;
#3384 = CARTESIAN_POINT ( 'NONE',  ( 12.22840589594397542, 30.63979685967524347, -5.723655948989013531 ) ) ;
#3385 = CARTESIAN_POINT ( 'NONE',  ( -12.00723429333529779, 56.16046608847325672, 6.256725284067366388 ) ) ;
#3386 = CARTESIAN_POINT ( 'NONE',  ( 8.343458848123583849, 53.87999999999999545, -11.48378591275253768 ) ) ;
#3387 = CARTESIAN_POINT ( 'NONE',  ( 9.174595195680133486, 33.03757788585047450, 9.903405154293709600 ) ) ;
#3388 = CARTESIAN_POINT ( 'NONE',  ( 4.913930544642371778, 43.00284194709907126, -12.57587111961252191 ) ) ;
#3389 = CARTESIAN_POINT ( 'NONE',  ( 11.94294432412099916, 39.66253801985712357, -6.294138039312064059 ) ) ;
#3390 = ORIENTED_EDGE ( 'NONE', *, *, #4854, .T. ) ;
#3391 = CARTESIAN_POINT ( 'NONE',  ( -13.24494331279968762, 61.83784905754306038, -2.611875526739312559 ) ) ;
#3392 = ORIENTED_EDGE ( 'NONE', *, *, #4542, .F. ) ;
#3393 = ORIENTED_EDGE ( 'NONE', *, *, #13130, .T. ) ;
#3394 = CARTESIAN_POINT ( 'NONE',  ( -8.549982208541774191E-16, 29.67999999999999972, 14.19474002721660355 ) ) ;
#3395 = CARTESIAN_POINT ( 'NONE',  ( 13.16986379960055054, -18.73124999999995666, -13.16986379959834430 ) ) ;
#3396 = CARTESIAN_POINT ( 'NONE',  ( 9.793712905158246329, 48.06848970801387111, 9.292869918114371686 ) ) ;
#3397 = CARTESIAN_POINT ( 'NONE',  ( 0.5920084214834188119, 58.15871356119428270, -13.50000000000000711 ) ) ;
#3398 = CARTESIAN_POINT ( 'NONE',  ( 7.095737324529082457, 78.91631958237633171, -11.48492378435084404 ) ) ;
#3399 = CARTESIAN_POINT ( 'NONE',  ( 9.520470885617715595, 79.13000000000000966, 6.917026985038134512 ) ) ;
#3400 = CARTESIAN_POINT ( 'NONE',  ( 13.50000000000000355, 38.57999999999999829, -4.386415899144233244 ) ) ;
#3401 = CARTESIAN_POINT ( 'NONE',  ( 12.39312577248542624, 2.367644581053835256E-15, 4.108133863307598332 ) ) ;
#3402 = CARTESIAN_POINT ( 'NONE',  ( -2.279876193866607892, 46.26197366689496704, -13.30632321474556434 ) ) ;
#3403 = LINE ( 'NONE', #8903, #5728 ) ;
#3404 = CARTESIAN_POINT ( 'NONE',  ( -4.711679271993003404, -47.90312499999986784, -11.37500000000039613 ) ) ;
#3405 = CARTESIAN_POINT ( 'NONE',  ( 10.47640949927847842, 54.10478805614472719, 8.515037930683744705 ) ) ;
#3406 = ORIENTED_EDGE ( 'NONE', *, *, #3832, .F. ) ;
#3407 = DIRECTION ( 'NONE',  ( -0.000000000000000000, -1.000000000000000000, -0.000000000000000000 ) ) ;
#3408 = EDGE_CURVE ( 'NONE', #10105, #13489, #2294, .T. ) ;
#3409 = ORIENTED_EDGE ( 'NONE', *, *, #17329, .T. ) ;
#3410 = CARTESIAN_POINT ( 'NONE',  ( 5.323009095788314937, 66.98734768220822389, -12.40627203521292721 ) ) ;
#3411 = CARTESIAN_POINT ( 'NONE',  ( -5.541662318619955840, 34.38103254278009757, -12.31017199372226223 ) ) ;
#3412 = CARTESIAN_POINT ( 'NONE',  ( -9.552639591052204498E-13, -79.08749999999980673, 11.37500000000000000 ) ) ;
#3413 = CARTESIAN_POINT ( 'NONE',  ( 8.000000000000023093, 0.000000000000000000, -17.32050807568876394 ) ) ;
#3414 = CARTESIAN_POINT ( 'NONE',  ( -3.609344227228918900, 59.55023083539120421, 13.00886259437187142 ) ) ;
#3415 = CARTESIAN_POINT ( 'NONE',  ( 16.17792858571907644, 8.007293667506182544, 8.349340579021683695 ) ) ;
#3416 = CARTESIAN_POINT ( 'NONE',  ( 11.00000000000001599, 0.000000000000000000, -15.58845726811988364 ) ) ;
#3417 = CARTESIAN_POINT ( 'NONE',  ( 13.37466002425821188, 72.36584947057816919, 1.835341461556227127 ) ) ;
#3418 = CARTESIAN_POINT ( 'NONE',  ( 8.048570524534548909, 66.87494734074847713, -10.83862139358550003 ) ) ;
#3419 = CARTESIAN_POINT ( 'NONE',  ( 2.279995255611139653E-15, 33.17999999999999972, -12.37355403259654985 ) ) ;
#3420 = CARTESIAN_POINT ( 'NONE',  ( -4.171729424061787483, 55.32999999999999829, -12.83926296998457417 ) ) ;
#3421 = CARTESIAN_POINT ( 'NONE',  ( -5.775258882854464204, 52.39010693232381755, -12.20232514914052402 ) ) ;
#3422 = CARTESIAN_POINT ( 'NONE',  ( -13.50000000000000000, 51.93000000000000682, -3.306546357697853733E-15 ) ) ;
#3423 = CARTESIAN_POINT ( 'NONE',  ( 13.50000000000000355, 77.57999999999999829, -4.386415899144233244 ) ) ;
#3424 = CARTESIAN_POINT ( 'NONE',  ( 7.272992578804311492, -3.120000000000004992, -10.01041549318726709 ) ) ;
#3425 = CARTESIAN_POINT ( 'NONE',  ( -1.650043268377658690, 68.62054052734106335, 13.40390642837740565 ) ) ;
#3426 = CARTESIAN_POINT ( 'NONE',  ( 18.62500000000064304, -17.69062499999995453, -7.714727599197335195 ) ) ;
#3427 = CYLINDRICAL_SURFACE ( 'NONE', #15772, 22.50000000000000355 ) ;
#3428 = CARTESIAN_POINT ( 'NONE',  ( -13.16986379960055231, -43.70624999999989768, 13.16986379959834252 ) ) ;
#3429 = CARTESIAN_POINT ( 'NONE',  ( -11.25052354211586270, 65.20990605257976824, 7.462422595341770659 ) ) ;
#3430 = CARTESIAN_POINT ( 'NONE',  ( 17.42428528562858148, 5.918584287042170544, -19.29752010712846300 ) ) ;
#3431 = LINE ( 'NONE', #3249, #2321 ) ;
#3432 = VERTEX_POINT ( 'NONE', #11952 ) ;
#3433 = CARTESIAN_POINT ( 'NONE',  ( -11.76794919243112325, 38.77999999999999403, -3.823638476888998827 ) ) ;
#3434 = DIRECTION ( 'NONE',  ( 0.000000000000000000, 0.000000000000000000, -1.000000000000000000 ) ) ;
#3435 = CARTESIAN_POINT ( 'NONE',  ( -4.741376437275918398, 40.35074587188617556, -12.64175464265864157 ) ) ;
#3436 = CARTESIAN_POINT ( 'NONE',  ( -12.96199357294905674, 31.79498504800923442, -3.773402922091955602 ) ) ;
#3437 = CARTESIAN_POINT ( 'NONE',  ( 5.450067102490391946, 74.87759374410906332, 12.35271490370261027 ) ) ;
#3438 = CARTESIAN_POINT ( 'NONE',  ( 10.92172942406178926, 62.13000000000000256, 7.935100905948387684 ) ) ;
#3439 = CIRCLE ( 'NONE', #9964, 4.000000000000000000 ) ;
#3440 = CARTESIAN_POINT ( 'NONE',  ( 690.7486963872879642, 776.4553902717702840, 1297.674793841596738 ) ) ;
#3441 = CARTESIAN_POINT ( 'NONE',  ( -5.491332954668864730, 30.39042612893359419, 16.75890910139807843 ) ) ;
#3442 = CARTESIAN_POINT ( 'NONE',  ( 11.68331733722775034, 51.68148845516454060, -6.763944398493564769 ) ) ;
#3443 = CARTESIAN_POINT ( 'NONE',  ( -13.32055366127931961, 38.00703768986679165, 2.194235484290746552 ) ) ;
#3444 = CARTESIAN_POINT ( 'NONE',  ( 11.94661826698584939, 36.66226039872729814, -6.287206104090115488 ) ) ;
#3445 = CARTESIAN_POINT ( 'NONE',  ( -8.043339635997652337, -17.65624999999997513, 8.043339635996300530 ) ) ;
#3446 = LINE ( 'NONE', #11324, #14177 ) ;
#3447 = CARTESIAN_POINT ( 'NONE',  ( -10.85718845775721064, 77.23369997451160884, 8.023478501512466110 ) ) ;
#3448 = CIRCLE ( 'NONE', #5155, 12.00000000000000178 ) ;
#3449 = EDGE_CURVE ( 'NONE', #6427, #15651, #14492, .T. ) ;
#3450 = LINE ( 'NONE', #793, #8473 ) ;
#3451 = CARTESIAN_POINT ( 'NONE',  ( 5.478462649124859141, 41.87859710647594369, 12.33842961194233290 ) ) ;
#3452 = CARTESIAN_POINT ( 'NONE',  ( 13.49272709919642566, 48.41445879050284873, 0.4520991473949109163 ) ) ;
#3453 = CARTESIAN_POINT ( 'NONE',  ( 11.76794919243112680, 14.57999999999999474, -3.823638476888993942 ) ) ;
#3454 = ORIENTED_EDGE ( 'NONE', *, *, #15559, .T. ) ;
#3455 = CARTESIAN_POINT ( 'NONE',  ( -9.520470885617715595, 62.63000000000000256, -6.917026985038136289 ) ) ;
#3456 = CARTESIAN_POINT ( 'NONE',  ( 8.043339635997652337, 5.168750000000006395, -8.043339635996304082 ) ) ;
#3457 = CARTESIAN_POINT ( 'NONE',  ( 11.37500000000000000, -99.89999999999976410, 0.000000000000000000 ) ) ;
#3458 = CARTESIAN_POINT ( 'NONE',  ( -13.49999999999999822, 2.079999999999997851, 4.386415899144235908 ) ) ;
#3459 = CARTESIAN_POINT ( 'NONE',  ( 7.272992578804311492, 29.88000000000000966, -10.01041549318726709 ) ) ;
#3460 = CARTESIAN_POINT ( 'NONE',  ( -8.380961239556755871, 80.92999999999997840, -9.227099233233150954 ) ) ;
#3461 = CARTESIAN_POINT ( 'NONE',  ( 18.62500000000000000, -49.94999999999988205, 1.560692158462880521E-12 ) ) ;
#3462 = CARTESIAN_POINT ( 'NONE',  ( 15.00000000000000000, -99.89999999999999147, 0.000000000000000000 ) ) ;
#3463 = CARTESIAN_POINT ( 'NONE',  ( 9.520470885617715595, 49.13000000000000256, 6.917026985038134512 ) ) ;
#3464 = VECTOR ( 'NONE', #10530, 1000.000000000000000 ) ;
#3465 = CARTESIAN_POINT ( 'NONE',  ( -13.46528334221770251, 58.96347564477174075, 0.9676412435863588346 ) ) ;
#3466 = CARTESIAN_POINT ( 'NONE',  ( 12.90801733370770954, 45.28818780823190338, 3.954641600816362956 ) ) ;
#3467 = CARTESIAN_POINT ( 'NONE',  ( 10.14775816985478230, 69.77298195707258799, -8.903540694107199727 ) ) ;
#3468 = CARTESIAN_POINT ( 'NONE',  ( 1.227614123976220384, 80.72414343316154373, 13.44515162415854803 ) ) ;
#3469 = CARTESIAN_POINT ( 'NONE',  ( 13.48837557053283831, 30.44930113163437824, -0.5606353105131218761 ) ) ;
#3470 = CARTESIAN_POINT ( 'NONE',  ( -13.49205171756009847, 55.94874241206034071, 0.5458872085021070353 ) ) ;
#3471 = CARTESIAN_POINT ( 'NONE',  ( -4.556504444975026047, 50.51610007432194749, 12.72330644818372214 ) ) ;
#3472 = DIRECTION ( 'NONE',  ( 0.000000000000000000, -1.000000000000000000, 0.000000000000000000 ) ) ;
#3473 = CARTESIAN_POINT ( 'NONE',  ( 0.2926259582140912641, 43.16951355705446502, -13.49726570074850152 ) ) ;
#3474 = CARTESIAN_POINT ( 'NONE',  ( 6.806927860051751544, 39.92851749465472722, -11.67113343977014672 ) ) ;
#3475 = EDGE_LOOP ( 'NONE', ( #8992, #1711, #8082, #15058 ) ) ;
#3476 = CARTESIAN_POINT ( 'NONE',  ( -10.77335659271368762, 61.62127811166998015, -8.136614450085879469 ) ) ;
#3477 = ORIENTED_EDGE ( 'NONE', *, *, #9399, .T. ) ;
#3478 = VERTEX_POINT ( 'NONE', #11692 ) ;
#3479 = CARTESIAN_POINT ( 'NONE',  ( -13.49999999999999822, 28.78000000000001535, -4.386415899144240349 ) ) ;
#3480 = CARTESIAN_POINT ( 'NONE',  ( -7.714727599200467800, -11.44687499999997371, 18.62499999999934630 ) ) ;
#3481 = CARTESIAN_POINT ( 'NONE',  ( 12.97866832662360537, 48.29713054261845429, 3.716351513807763407 ) ) ;
#3482 = CARTESIAN_POINT ( 'NONE',  ( 11.37239215724911112, 57.70229078515689025, -7.275958244018569943 ) ) ;
#3483 = CARTESIAN_POINT ( 'NONE',  ( 6.873487081399273002, 78.92563002817296081, -11.61942495236515249 ) ) ;
#3484 = CARTESIAN_POINT ( 'NONE',  ( 9.520470885617717371, 79.72999999999998977, -6.917026985038131848 ) ) ;
#3485 = CARTESIAN_POINT ( 'NONE',  ( 5.441113646577305119, 5.918584287042172321, 25.42428528562857792 ) ) ;
#3486 = EDGE_CURVE ( 'NONE', #10721, #6584, #2947, .T. ) ;
#3487 = CARTESIAN_POINT ( 'NONE',  ( 11.06573348676161217, -99.99999999999995737, 3.020779226708963261 ) ) ;
#3488 = FACE_OUTER_BOUND ( 'NONE', #15893, .T. ) ;
#3489 = CARTESIAN_POINT ( 'NONE',  ( -4.711679271993003404, -14.60312499999994706, -11.37500000000039613 ) ) ;
#3490 = CARTESIAN_POINT ( 'NONE',  ( 12.00000000000000178, 5.146025403784437735, 3.899036354794877202 ) ) ;
#3491 = CARTESIAN_POINT ( 'NONE',  ( 6.074345959363277814, 33.95809426174932355, -12.05647970507914302 ) ) ;
#3492 = ORIENTED_EDGE ( 'NONE', *, *, #7896, .T. ) ;
#3493 = PLANE ( 'NONE',  #14007 ) ;
#3494 = ORIENTED_EDGE ( 'NONE', *, *, #11716, .T. ) ;
#3495 = CARTESIAN_POINT ( 'NONE',  ( 17.32050807568878170, 7.773118517290099838, -7.999999999999961808 ) ) ;
#3496 = CARTESIAN_POINT ( 'NONE',  ( -4.711679271993004292, -88.45312499999978684, -11.37500000000039435 ) ) ;
#3497 = CARTESIAN_POINT ( 'NONE',  ( 19.29752010712851984, 0.000000000000000000, -17.42428528562851042 ) ) ;
#3498 = CARTESIAN_POINT ( 'NONE',  ( -7.075555937736629275, 59.41716819547789186, 11.49737106684309751 ) ) ;
#3499 = DIRECTION ( 'NONE',  ( -1.000000000000000000, 0.000000000000000000, 4.676985943005715098E-16 ) ) ;
#3500 = DIRECTION ( 'NONE',  ( 1.000000000000000000, 0.000000000000000000, 0.000000000000000000 ) ) ;
#3501 = CARTESIAN_POINT ( 'NONE',  ( 7.829317792819562527, 71.97528757275648559, 10.99897765872064781 ) ) ;
#3502 = CARTESIAN_POINT ( 'NONE',  ( -8.343458848123576743, 52.47999999999999687, -11.48378591275254301 ) ) ;
#3503 = CARTESIAN_POINT ( 'NONE',  ( -6.381350698036120761, 52.41419776773467731, -11.90580418029937526 ) ) ;
#3504 = EDGE_CURVE ( 'NONE', #3760, #15564, #8965, .T. ) ;
#3505 = CARTESIAN_POINT ( 'NONE',  ( 10.92172942406178926, 77.13000000000000966, 7.935100905948387684 ) ) ;
#3506 = CARTESIAN_POINT ( 'NONE',  ( -1.564113515457998572E-12, -62.43749999999985079, 18.62500000000000000 ) ) ;
#3507 = CARTESIAN_POINT ( 'NONE',  ( -8.574308837607619083, 68.35095914637041403, 10.42743186381050968 ) ) ;
#3508 = CARTESIAN_POINT ( 'NONE',  ( -1.564113515457998572E-12, -62.43749999999985079, 18.62500000000000000 ) ) ;
#3509 = DIRECTION ( 'NONE',  ( 0.000000000000000000, -1.000000000000000000, 0.000000000000000000 ) ) ;
#3510 = CARTESIAN_POINT ( 'NONE',  ( 18.62499999999934630, -15.60937499999996270, 7.714727599200467800 ) ) ;
#3511 = CARTESIAN_POINT ( 'NONE',  ( -0.6046803220343888174, 65.65828050903189705, 13.49999999993799982 ) ) ;
#3512 = CARTESIAN_POINT ( 'NONE',  ( 0.000000000000000000, 0.000000000000000000, 9.500000000000021316 ) ) ;
#3513 = AXIS2_PLACEMENT_3D ( 'NONE', #16928, #11726, #10235 ) ;
#3514 = CARTESIAN_POINT ( 'NONE',  ( -1.005545769327274827E-13, 2.180000000000013927, -13.50000000000000000 ) ) ;
#3515 = ORIENTED_EDGE ( 'NONE', *, *, #53, .F. ) ;
#3516 = CARTESIAN_POINT ( 'NONE',  ( 11.76794919243112325, 31.27999999999998693, 3.823638476888997051 ) ) ;
#3517 = CARTESIAN_POINT ( 'NONE',  ( -4.273851079481598703, 40.33368115456159586, -12.80566632602802102 ) ) ;
#3518 = CARTESIAN_POINT ( 'NONE',  ( -13.41444007591816678, 31.98338318546857550, 1.533229712954465196 ) ) ;
#3519 = CARTESIAN_POINT ( 'NONE',  ( -22.26874168100106033, 6.548282979925672542, -8.000000000000257572 ) ) ;
#3520 = CARTESIAN_POINT ( 'NONE',  ( 13.06329500387617770, 60.30866768971296921, 3.406192448351748503 ) ) ;
#3521 = DIRECTION ( 'NONE',  ( 0.000000000000000000, 1.000000000000000000, 0.000000000000000000 ) ) ;
#3522 = CARTESIAN_POINT ( 'NONE',  ( -4.171729424061787483, 78.32999999999999829, -12.83926296998457417 ) ) ;
#3523 = ADVANCED_FACE ( 'NONE', ( #6397 ), #15641, .F. ) ;
#3524 = CARTESIAN_POINT ( 'NONE',  ( 13.49059967034253305, 51.44733065808145511, -0.5037421684802066979 ) ) ;
#3525 = CARTESIAN_POINT ( 'NONE',  ( -13.48070957841285278, 37.90502422016587047, -0.7223451569848480247 ) ) ;
#3526 = CARTESIAN_POINT ( 'NONE',  ( 11.22475465503331371, 36.71175793279847710, -7.500328621267835061 ) ) ;
#3527 = CARTESIAN_POINT ( 'NONE',  ( -9.552639591052204498E-13, -36.38749999999993179, 11.37499999999999645 ) ) ;
#3528 = CARTESIAN_POINT ( 'NONE',  ( 8.378360550312208943, 10.00007452681958497, 10.58551248116806498 ) ) ;
#3529 = DIRECTION ( 'NONE',  ( -1.734723475976807094E-16, 1.000000000000000000, 0.000000000000000000 ) ) ;
#3530 = CARTESIAN_POINT ( 'NONE',  ( -1.551070049701340103, 80.62418276194892997, 13.41104721329206839 ) ) ;
#3531 = CARTESIAN_POINT ( 'NONE',  ( 5.633694881767536522, 41.88459927968532526, 12.26853111873423252 ) ) ;
#3532 = CARTESIAN_POINT ( 'NONE',  ( 13.46307399052660259, 48.39473455737326901, 1.018718451003600478 ) ) ;
#3533 = CARTESIAN_POINT ( 'NONE',  ( -3.636496289402156190, 10.53000000000001180, 11.19198476289190758 ) ) ;
#3534 = VERTEX_POINT ( 'NONE', #17069 ) ;
#3535 = CARTESIAN_POINT ( 'NONE',  ( -7.576616670048093940E-16, 60.67999999999999261, 12.37355403259654807 ) ) ;
#3536 = CARTESIAN_POINT ( 'NONE',  ( 8.043339635996302306, -7.318749999999964118, 8.043339635997654113 ) ) ;
#3537 = DIRECTION ( 'NONE',  ( 0.000000000000000000, 0.000000000000000000, -1.000000000000000000 ) ) ;
#3538 = CARTESIAN_POINT ( 'NONE',  ( -8.343458848123576743, 1.479999999999995541, -11.48378591275254301 ) ) ;
#3539 = B_SPLINE_CURVE_WITH_KNOTS ( 'NONE', 3,
 ( #14571, #11682, #13088, #9041 ),
 .UNSPECIFIED., .F., .F.,
 ( 4, 4 ),
 ( 0.008786844460939030252, 0.01643317035798799036 ),
 .UNSPECIFIED. ) ;
#3540 = CARTESIAN_POINT ( 'NONE',  ( 3.636496289402154414, 31.82999999999999829, 11.19198476289190758 ) ) ;
#3541 = CARTESIAN_POINT ( 'NONE',  ( 0.5390086576906194527, 76.16062051171672920, -13.49046569834956877 ) ) ;
#3542 = CARTESIAN_POINT ( 'NONE',  ( -7.714727599197334307, -88.45312499999977263, -18.62500000000064304 ) ) ;
#3543 = CARTESIAN_POINT ( 'NONE',  ( 13.50000000000000000, 81.43000000000000682, 1.653273178848926867E-15 ) ) ;
#3544 = CIRCLE ( 'NONE', #728, 12.00000000000000178 ) ;
#3545 = CARTESIAN_POINT ( 'NONE',  ( -9.520470885617717371, 51.22999999999999687, 6.917026985038133624 ) ) ;
#3546 = DIRECTION ( 'NONE',  ( 0.8660221325896413358, 0.000000000000000000, -0.5000056658327882708 ) ) ;
#3547 = EDGE_CURVE ( 'NONE', #10228, #6792, #12433, .T. ) ;
#3548 = CARTESIAN_POINT ( 'NONE',  ( -13.47664760107280735, 58.90259797499196281, -0.7937112629172573541 ) ) ;
#3549 = CARTESIAN_POINT ( 'NONE',  ( 10.82628732869974719, 45.12415098472465758, 8.070053677659583258 ) ) ;
#3550 = CARTESIAN_POINT ( 'NONE',  ( 13.09907156312732290, 69.54612857034256024, -3.265651416783837746 ) ) ;
#3551 = CARTESIAN_POINT ( 'NONE',  ( 4.572122312880307682, 80.84449485487320430, 12.70468199279591559 ) ) ;
#3552 = CARTESIAN_POINT ( 'NONE',  ( 13.06123906118353517, 30.55161712359772253, -3.413860246534342835 ) ) ;
#3553 = CARTESIAN_POINT ( 'NONE',  ( -13.45979128135589420, 55.89390028866353788, -1.044999607113579643 ) ) ;
#3554 = CARTESIAN_POINT ( 'NONE',  ( -13.49470981577344375, 49.91485972376758440, -0.4364497393623030241 ) ) ;
#3555 = FACE_OUTER_BOUND ( 'NONE', #581, .T. ) ;
#3556 = CARTESIAN_POINT ( 'NONE',  ( 1.137810555388867773, -1.046521029022079216E-15, -11.94593600937347055 ) ) ;
#3557 = CARTESIAN_POINT ( 'NONE',  ( 13.41230998493642623, 39.48517279672220326, -1.584139233609136665 ) ) ;
#3558 = ORIENTED_EDGE ( 'NONE', *, *, #11641, .F. ) ;
#3559 = CARTESIAN_POINT ( 'NONE',  ( -5.845759849409800424, 61.39277117633377401, -12.17771138739238701 ) ) ;
#3560 = CARTESIAN_POINT ( 'NONE',  ( -9.520470885617715595, 6.629999999999997229, -6.917026985038136289 ) ) ;
#3561 = ORIENTED_EDGE ( 'NONE', *, *, #2631, .T. ) ;
#3562 = ORIENTED_EDGE ( 'NONE', *, *, #7310, .F. ) ;
#3563 = CARTESIAN_POINT ( 'NONE',  ( 8.343458848123583849, 27.88000000000001322, -11.48378591275253768 ) ) ;
#3564 = CARTESIAN_POINT ( 'NONE',  ( 1.561832610794586538E-12, -4.162499999999989875, -18.62500000000000000 ) ) ;
#3565 = CARTESIAN_POINT ( 'NONE',  ( 6.813825994921812068, 47.93197876211288389, 11.65439317571491706 ) ) ;
#3566 = CARTESIAN_POINT ( 'NONE',  ( 10.68081498587143408, 57.74381789421609312, -8.257788020075247815 ) ) ;
#3567 = CARTESIAN_POINT ( 'NONE',  ( 0.7009303126130895789, 79.15481186450742257, -13.48240536218643193 ) ) ;
#3568 = CARTESIAN_POINT ( 'NONE',  ( -11.76794919243112325, 75.08000000000001251, 3.823638476888994386 ) ) ;
#3569 = CARTESIAN_POINT ( 'NONE',  ( 11.76794919243112325, 82.43000000000000682, 1.441158131103945434E-15 ) ) ;
#3570 = CARTESIAN_POINT ( 'NONE',  ( 0.000000000000000000, 30.93000000000001393, 0.000000000000000000 ) ) ;
#3571 = CIRCLE ( 'NONE', #10639, 13.50000000000000000 ) ;
#3572 = SURFACE_STYLE_USAGE ( .BOTH. , #831 ) ;
#3573 = DIRECTION ( 'NONE',  ( -0.000000000000000000, 1.000000000000000000, -0.000000000000000000 ) ) ;
#3574 = CARTESIAN_POINT ( 'NONE',  ( 8.043339635996302306, -57.26874999999984794, 8.043339635997654113 ) ) ;
#3575 = CARTESIAN_POINT ( 'NONE',  ( 8.343458848123580296, 43.97999999999999687, 11.48378591275253768 ) ) ;
#3576 = DIRECTION ( 'NONE',  ( 0.000000000000000000, 0.000000000000000000, -1.000000000000000000 ) ) ;
#3577 = ORIENTED_EDGE ( 'NONE', *, *, #11185, .T. ) ;
#3578 = FACE_OUTER_BOUND ( 'NONE', #3654, .T. ) ;
#3579 = ORIENTED_EDGE ( 'NONE', *, *, #1090, .T. ) ;
#3580 = CARTESIAN_POINT ( 'NONE',  ( 9.538709233711902776E-13, -44.71249999999991331, -11.37499999999999645 ) ) ;
#3581 = EDGE_CURVE ( 'NONE', #8520, #860, #15587, .T. ) ;
#3582 = CARTESIAN_POINT ( 'NONE',  ( 0.4449454661118308341, 77.69610243158906826, 13.49999999997334044 ) ) ;
#3583 = CARTESIAN_POINT ( 'NONE',  ( -1.328659818498353332E-07, 59.67999629905246195, 13.49999999999999822 ) ) ;
#3584 = CARTESIAN_POINT ( 'NONE',  ( 7.500000000000000888, -22.00000000000000000, 9.367496997597600128 ) ) ;
#3585 = FACE_OUTER_BOUND ( 'NONE', #16444, .T. ) ;
#3586 = CARTESIAN_POINT ( 'NONE',  ( 0.000000000000000000, -100.0000000000000000, 0.000000000000000000 ) ) ;
#3587 = CARTESIAN_POINT ( 'NONE',  ( 10.92172942406179104, 48.72999999999999687, -7.935100905948385908 ) ) ;
#3588 = CARTESIAN_POINT ( 'NONE',  ( -4.378381081909518358, 71.52253779549604928, 12.77041120775835026 ) ) ;
#3589 = FILL_AREA_STYLE ('',( #7769 ) ) ;
#3590 = CARTESIAN_POINT ( 'NONE',  ( 2.000520122481862502E-14, 76.67999999999999261, 13.50000000000000000 ) ) ;
#3591 = CARTESIAN_POINT ( 'NONE',  ( -18.62499999999934985, -57.23437499999987921, -7.714727599200458918 ) ) ;
#3592 = CARTESIAN_POINT ( 'NONE',  ( -0.9445818373508010346, 68.64612565221730733, 13.46771734312773638 ) ) ;
#3593 = CARTESIAN_POINT ( 'NONE',  ( -18.62499999999934985, -23.93437499999993889, -7.714727599200458918 ) ) ;
#3594 = CARTESIAN_POINT ( 'NONE',  ( 3.280605613281809330, 55.06204156931236326, -13.09532926545062814 ) ) ;
#3595 = CARTESIAN_POINT ( 'NONE',  ( -13.16986379960055231, -60.35624999999985363, 13.16986379959834252 ) ) ;
#3596 = CARTESIAN_POINT ( 'NONE',  ( -9.675226902770793558, 65.29754703176814701, 9.415198896858003152 ) ) ;
#3597 = DIRECTION ( 'NONE',  ( 0.8660254037844362651, 0.000000000000000000, 0.5000000000000041078 ) ) ;
#3598 = CARTESIAN_POINT ( 'NONE',  ( -4.672525169807293821, 35.51179140871166595, 12.66707033060281518 ) ) ;
#3599 = CARTESIAN_POINT ( 'NONE',  ( 13.50000000000000355, 25.58000000000000185, -4.386415899144233244 ) ) ;
#3600 = EDGE_CURVE ( 'NONE', #8166, #1772, #5243, .T. ) ;
#3601 = ORIENTED_EDGE ( 'NONE', *, *, #14970, .T. ) ;
#3602 = DIRECTION ( 'NONE',  ( 0.5000000000000066613, -0.000000000000000000, -0.8660254037844347108 ) ) ;
#3603 = CARTESIAN_POINT ( 'NONE',  ( 1.108954987895778950E-11, 4.813974596216015200, 12.00000000000000178 ) ) ;
#3604 = CARTESIAN_POINT ( 'NONE',  ( 2.138189944381238661, 79.75688142232024802, 13.50000000000000000 ) ) ;
#3605 = CARTESIAN_POINT ( 'NONE',  ( -13.46812497729234259, 31.89793320150942435, -0.9275556759729549627 ) ) ;
#3606 = CARTESIAN_POINT ( 'NONE',  ( -3.556480217745532916E-14, 9.046025403784437202, -12.00000000000000000 ) ) ;
#3607 = CARTESIAN_POINT ( 'NONE',  ( 13.50000640706135613, 60.42933411119164333, 0.01923106255287391694 ) ) ;
#3608 = CARTESIAN_POINT ( 'NONE',  ( -8.549982208541774191E-16, 6.679999999999998828, 14.19474002721660355 ) ) ;
#3609 = CARTESIAN_POINT ( 'NONE',  ( -9.925458028546751521, 53.28467197136558298, 9.150698730621169119 ) ) ;
#3610 = CARTESIAN_POINT ( 'NONE',  ( -7.576616670048093940E-16, 60.67999999999998550, 12.37355403259654985 ) ) ;
#3611 = CARTESIAN_POINT ( 'NONE',  ( 13.41279326728364651, 51.37661727247101595, 1.532238328333574096 ) ) ;
#3612 = CARTESIAN_POINT ( 'NONE',  ( -12.57861966457431002, 38.10786478379095854, 4.901884260589575604 ) ) ;
#3613 = CARTESIAN_POINT ( 'NONE',  ( 13.47639277022257964, 36.45819009604027627, -0.8166540340939039133 ) ) ;
#3614 = CARTESIAN_POINT ( 'NONE',  ( 4.711679271994911211, -60.32187499999988489, -11.37499999999960210 ) ) ;
#3615 = CARTESIAN_POINT ( 'NONE',  ( 12.00000000000000178, 2.146025403784442620, 3.899036354794877202 ) ) ;
#3616 = CARTESIAN_POINT ( 'NONE',  ( -10.66312149623454530, 77.24479860351357274, 8.279365195195687477 ) ) ;
#3617 = CARTESIAN_POINT ( 'NONE',  ( -4.905989025644352353, 80.50308446184858724, 12.57886947468737482 ) ) ;
#3618 = CARTESIAN_POINT ( 'NONE',  ( 7.500000000000000000, 105.3828822090421227, -8.693347190813733860 ) ) ;
#3619 = ORIENTED_EDGE ( 'NONE', *, *, #13412, .T. ) ;
#3620 = CARTESIAN_POINT ( 'NONE',  ( -11.76794919243112325, 9.929999999999994387, -2.602085213965210642E-15 ) ) ;
#3621 = ORIENTED_EDGE ( 'NONE', *, *, #10800, .T. ) ;
#3622 = CARTESIAN_POINT ( 'NONE',  ( -11.76794919243112325, 56.77999999999998693, -3.823638476888998827 ) ) ;
#3623 = CARTESIAN_POINT ( 'NONE',  ( 11.37500000000039435, -1.040624999999997025, -4.711679271993004292 ) ) ;
#3624 = CARTESIAN_POINT ( 'NONE',  ( -4.711679271993003404, -88.45312499999977263, -11.37500000000039435 ) ) ;
#3625 = CARTESIAN_POINT ( 'NONE',  ( 8.343458848123583849, 0.8799999999999997824, -11.48378591275253768 ) ) ;
#3626 = EDGE_CURVE ( 'NONE', #4018, #4394, #13707, .T. ) ;
#3627 = CARTESIAN_POINT ( 'NONE',  ( 10.51572120785151654, 75.75302732738094846, -8.465820318027104108 ) ) ;
#3628 = CARTESIAN_POINT ( 'NONE',  ( -3.636496289402155746, 33.52999999999999403, 11.19198476289190936 ) ) ;
#3629 = VECTOR ( 'NONE', #16184, 1000.000000000000000 ) ;
#3630 = CARTESIAN_POINT ( 'NONE',  ( 1.561832610794586538E-12, -70.76249999999983231, -18.62500000000000000 ) ) ;
#3631 = CARTESIAN_POINT ( 'NONE',  ( 3.112499768079701745, 65.79190412735221116, 13.13630053735090542 ) ) ;
#3632 = CARTESIAN_POINT ( 'NONE',  ( -10.92172942406179104, 71.23000000000000398, 7.935100905948387684 ) ) ;
#3633 = CARTESIAN_POINT ( 'NONE',  ( -11.76794919243112325, 47.92999999999999972, -2.882316262207890869E-15 ) ) ;
#3634 = CARTESIAN_POINT ( 'NONE',  ( -1.900613283901089634, 9.390856018536133831, -11.99999999999790390 ) ) ;
#3635 = CARTESIAN_POINT ( 'NONE',  ( -13.46720615212894501, 58.96252600434252145, 0.9405017376672494267 ) ) ;
#3636 = CARTESIAN_POINT ( 'NONE',  ( 11.47344028360550006, 45.16420593273019080, 7.114091049973444214 ) ) ;
#3637 = CARTESIAN_POINT ( 'NONE',  ( 11.01362784260440542, 69.72461688776509448, -7.807153119340634717 ) ) ;
#3638 = DIRECTION ( 'NONE',  ( 0.8660254037844430375, -0.000000000000000000, -0.4999999999999925060 ) ) ;
#3639 = CARTESIAN_POINT ( 'NONE',  ( 13.48964992093387849, 30.44819364669021766, -0.5286683032485781641 ) ) ;
#3640 = AXIS2_PLACEMENT_3D ( 'NONE', #13459, #10911, #4096 ) ;
#3641 = CARTESIAN_POINT ( 'NONE',  ( -11.04618422503944686, 55.63728354584706182, -7.761965573417075603 ) ) ;
#3642 = CARTESIAN_POINT ( 'NONE',  ( -9.907659367957414531, 50.28597023960409018, 9.180989528200973027 ) ) ;
#3643 = CARTESIAN_POINT ( 'NONE',  ( 5.351965053708911846, 63.98625261907654505, -12.39380797406724710 ) ) ;
#3644 = FACE_OUTER_BOUND ( 'NONE', #7385, .T. ) ;
#3645 = CARTESIAN_POINT ( 'NONE',  ( 13.31289339363439517, 39.35132640896662082, 2.239837115172842896 ) ) ;
#3646 = EDGE_LOOP ( 'NONE', ( #9521, #7185, #17362, #8949 ) ) ;
#3647 = CARTESIAN_POINT ( 'NONE',  ( -9.584052401572662916, 70.55787012011465720, -9.510499048535340449 ) ) ;
#3648 = CARTESIAN_POINT ( 'NONE',  ( -10.86637700757906622, 61.62663672810896998, -8.012531335975232594 ) ) ;
#3649 =( BOUNDED_CURVE ( )  B_SPLINE_CURVE ( 2, ( #13265, #9223, #10623, #16158, #2548, #13179, #11863, #17238, #5148, #9395, #7978, #14575, #16074 ),
 .UNSPECIFIED., .F., .F. ) 
 B_SPLINE_CURVE_WITH_KNOTS ( ( 3, 2, 2, 2, 2, 2, 3 ),
 ( 0.2916666666666666297, 0.2944444444444444531, 0.2999999999999999889, 0.3055555555555555802, 0.3111111111111111160, 0.3166666666666666519, 0.3194444444444444198 ),
 .UNSPECIFIED. ) 
 CURVE ( )  GEOMETRIC_REPRESENTATION_ITEM ( )  RATIONAL_B_SPLINE_CURVE ( ( 0.9755282581475768211, 0.9755282581475765991, 1.000000000000000000, 0.9510565162951535312, 1.000000000000000000, 0.9510565162951535312, 1.000000000000000000, 0.9510565162951535312, 1.000000000000000000, 0.9510565162951535312, 1.000000000000000000, 0.9755282581475770431, 0.9755282581475768211 ) ) 
 REPRESENTATION_ITEM ( '' )  );
#3650 = CARTESIAN_POINT ( 'NONE',  ( 11.76794919243112325, 8.280000000000006466, 3.823638476888996163 ) ) ;
#3651 = ORIENTED_EDGE ( 'NONE', *, *, #5434, .T. ) ;
#3652 = EDGE_CURVE ( 'NONE', #3044, #16628, #16079, .T. ) ;
#3653 = CARTESIAN_POINT ( 'NONE',  ( -11.54462091828690440, 40.66874641531683210, -7.004015811786465484 ) ) ;
#3654 = EDGE_LOOP ( 'NONE', ( #670, #11374, #7882 ) ) ;
#3655 = CARTESIAN_POINT ( 'NONE',  ( -4.171729424061787483, 25.33000000000001961, -12.83926296998457417 ) ) ;
#3656 = CARTESIAN_POINT ( 'NONE',  ( -18.62499999999934985, -7.284374999999982947, -7.714727599200458918 ) ) ;
#3657 = CARTESIAN_POINT ( 'NONE',  ( 2.254128362010559439, 47.76103611355556211, 13.31951350158262315 ) ) ;
#3658 = CARTESIAN_POINT ( 'NONE',  ( 1.938283894950695974, 58.11032032463412378, -13.36127657765577759 ) ) ;
#3659 = CARTESIAN_POINT ( 'NONE',  ( 12.18688363209133030, 78.64319475361247669, -5.807748549134894134 ) ) ;
#3660 = AXIS2_PLACEMENT_3D ( 'NONE', #14202, #6017, #16772 ) ;
#3661 = CARTESIAN_POINT ( 'NONE',  ( 2.272985001014427788E-15, 74.17999999999997840, -12.37355403259654985 ) ) ;
#3662 = CARTESIAN_POINT ( 'NONE',  ( 3.636496289402154414, 81.82999999999999829, 11.19198476289190936 ) ) ;
#3663 = FACE_OUTER_BOUND ( 'NONE', #13105, .T. ) ;
#3664 = CARTESIAN_POINT ( 'NONE',  ( 8.318912088914551362, -99.99999999999994316, 8.890191110864586577 ) ) ;
#3665 = CARTESIAN_POINT ( 'NONE',  ( -0.1635035910697570927, 67.18587897178171886, -13.49901470174091855 ) ) ;
#3666 = CARTESIAN_POINT ( 'NONE',  ( -11.37499999999960743, -49.98437499999987210, -4.711679271994912099 ) ) ;
#3667 = CARTESIAN_POINT ( 'NONE',  ( 19.29752010712840615, 0.000000000000000000, 17.42428528562864898 ) ) ;
#3668 = CARTESIAN_POINT ( 'NONE',  ( 3.496867611406847764, 34.05434841121682155, -13.04155495172319768 ) ) ;
#3669 = CARTESIAN_POINT ( 'NONE',  ( -13.48700498846246276, 73.90959446758982665, -0.5924077624709760403 ) ) ;
#3670 = ORIENTED_EDGE ( 'NONE', *, *, #16344, .T. ) ;
#3671 = ORIENTED_EDGE ( 'NONE', *, *, #14702, .F. ) ;
#3672 = DIRECTION ( 'NONE',  ( -1.000000000000000000, -8.862145109134287319E-17, 0.000000000000000000 ) ) ;
#3673 = ORIENTED_EDGE ( 'NONE', *, *, #14015, .T. ) ;
#3674 = CARTESIAN_POINT ( 'NONE',  ( -4.711679271994916540, -94.69687499999979252, 11.37499999999960210 ) ) ;
#3675 = CARTESIAN_POINT ( 'NONE',  ( -3.426950242872616847, 44.55682256194640445, 13.06444397049863504 ) ) ;
#3676 = CARTESIAN_POINT ( 'NONE',  ( -7.506691621707916262, 59.39882663589411749, 11.22238440737102749 ) ) ;
#3677 = DIRECTION ( 'NONE',  ( 8.673617379884035472E-17, -1.000000000000000000, 0.000000000000000000 ) ) ;
#3678 = DIRECTION ( 'NONE',  ( 0.000000000000000000, 0.000000000000000000, -1.000000000000000000 ) ) ;
#3679 = CARTESIAN_POINT ( 'NONE',  ( -8.343458848123576743, 55.47999999999998977, -11.48378591275254301 ) ) ;
#3680 = CARTESIAN_POINT ( 'NONE',  ( -7.866213445538476456, 71.38314426818901381, 10.97589501671720491 ) ) ;
#3681 = CIRCLE ( 'NONE', #10198, 12.00000000000000178 ) ;
#3682 = CARTESIAN_POINT ( 'NONE',  ( -9.432230830578065550, 59.31010286422545619, 9.668454110407326496 ) ) ;
#3683 = CARTESIAN_POINT ( 'NONE',  ( -7.714727599197335195, -55.15312499999986784, -18.62500000000064304 ) ) ;
#3684 = ADVANCED_FACE ( 'NONE', ( #12118 ), #16346, .T. ) ;
#3685 = CARTESIAN_POINT ( 'NONE',  ( 6.123233995736765296E-16, 75.00000000000000000, -5.000000000000000000 ) ) ;
#3686 = CARTESIAN_POINT ( 'NONE',  ( -18.62499999999934985, -73.88437499999982094, -7.714727599200458918 ) ) ;
#3687 = CARTESIAN_POINT ( 'NONE',  ( 6.762232371920031682, 54.93041419438679185, -11.69278108536045302 ) ) ;
#3688 = CARTESIAN_POINT ( 'NONE',  ( 9.520470885617717371, 20.72999999999999687, -6.917026985038131848 ) ) ;
#3689 = CARTESIAN_POINT ( 'NONE',  ( 13.16986379959834075, -47.86874999999988489, 13.16986379960055231 ) ) ;
#3690 = CARTESIAN_POINT ( 'NONE',  ( -7.991773808256851019, 65.37750511056809444, 10.88130972677807229 ) ) ;
#3691 = DIRECTION ( 'NONE',  ( 0.000000000000000000, 0.000000000000000000, -1.000000000000000000 ) ) ;
#3692 = CARTESIAN_POINT ( 'NONE',  ( -1.717771643151318361, 35.61820511656272004, 13.39054620278180430 ) ) ;
#3693 = CARTESIAN_POINT ( 'NONE',  ( 10.92172942406179104, 22.73000000000000043, -7.935100905948385908 ) ) ;
#3694 = ORIENTED_EDGE ( 'NONE', *, *, #15310, .F. ) ;
#3695 = CARTESIAN_POINT ( 'NONE',  ( 8.343458848123583849, 50.87999999999999545, -11.48378591275253768 ) ) ;
#3696 = CARTESIAN_POINT ( 'NONE',  ( -12.69323189075679359, 32.09621662746886983, 4.598406620704597714 ) ) ;
#3697 = CARTESIAN_POINT ( 'NONE',  ( -3.737279461696752201E-15, 73.17999999999999261, -13.50000000000000000 ) ) ;
#3698 = CARTESIAN_POINT ( 'NONE',  ( 9.443557525633938354, 60.05081174560719859, 9.647429353757006609 ) ) ;
#3699 = CARTESIAN_POINT ( 'NONE',  ( -13.49999999999999822, -6.220000000000002416, -4.386415899144240349 ) ) ;
#3700 = CARTESIAN_POINT ( 'NONE',  ( -11.98718778898151349, 53.15915301820461281, 6.209526914751407389 ) ) ;
#3701 = CARTESIAN_POINT ( 'NONE',  ( -9.520470885617717371, 60.22999999999999687, 6.917026985038133624 ) ) ;
#3702 = CARTESIAN_POINT ( 'NONE',  ( 13.37713670579460157, 51.36639808551130670, 1.819116265251073283 ) ) ;
#3703 = CARTESIAN_POINT ( 'NONE',  ( -13.47376594344626177, 37.90094777547172811, -0.8416043350724276007 ) ) ;
#3704 = CARTESIAN_POINT ( 'NONE',  ( 11.25768462558175287, 36.70972676642409027, -7.450841025583892829 ) ) ;
#3705 = CARTESIAN_POINT ( 'NONE',  ( 9.538709233711902776E-13, -28.06249999999995381, -11.37499999999999645 ) ) ;
#3706 = CARTESIAN_POINT ( 'NONE',  ( -4.145437653765961628, 74.53085911066104075, 12.85327900485357233 ) ) ;
#3707 = CARTESIAN_POINT ( 'NONE',  ( -8.225025902617534967, 77.36731451037184115, 10.71433264759214588 ) ) ;
#3708 = CARTESIAN_POINT ( 'NONE',  ( -6.694905124455936551, 80.43301383616126543, 11.72313240434259463 ) ) ;
#3709 = DIRECTION ( 'NONE',  ( 0.000000000000000000, 0.000000000000000000, 1.000000000000000000 ) ) ;
#3710 = ORIENTED_EDGE ( 'NONE', *, *, #9973, .T. ) ;
#3711 = CARTESIAN_POINT ( 'NONE',  ( 3.636496289402157078, 9.030000000000010019, -11.19198476289190936 ) ) ;
#3712 = EDGE_LOOP ( 'NONE', ( #13957, #7098, #10577, #7311 ) ) ;
#3713 = CARTESIAN_POINT ( 'NONE',  ( 11.76794919243112325, 55.27999999999998693, 3.823638476888997051 ) ) ;
#3714 = CARTESIAN_POINT ( 'NONE',  ( 4.711679271994911211, -62.47187499999984084, -11.37499999999960743 ) ) ;
#3715 = DIRECTION ( 'NONE',  ( 0.000000000000000000, 1.000000000000000000, 0.000000000000000000 ) ) ;
#3716 = CARTESIAN_POINT ( 'NONE',  ( 10.92172942406179104, 0.7300000000000084199, -7.935100905948385908 ) ) ;
#3717 = AXIS2_PLACEMENT_3D ( 'NONE', #14310, #13002, #9220 ) ;
#3718 = CARTESIAN_POINT ( 'NONE',  ( 6.226471401687747154, 75.95203426803303159, -11.97835911601103120 ) ) ;
#3719 = CARTESIAN_POINT ( 'NONE',  ( 9.235079662642815990, 32.03187319105528985, 10.25657514373247992 ) ) ;
#3720 = CARTESIAN_POINT ( 'NONE',  ( 8.343458848123583849, 75.87999999999998124, -11.48378591275253768 ) ) ;
#3721 = CARTESIAN_POINT ( 'NONE',  ( 9.520470885617715595, 43.13000000000000256, 6.917026985038134512 ) ) ;
#3722 = PLANE ( 'NONE',  #6954 ) ;
#3723 = CARTESIAN_POINT ( 'NONE',  ( -13.39844892242865626, 58.87026394863372758, -1.714548835752056632 ) ) ;
#3724 = EDGE_CURVE ( 'NONE', #10745, #3120, #12992, .T. ) ;
#3725 = CARTESIAN_POINT ( 'NONE',  ( 9.182243949852553655, 45.03795070569126580, 9.896291786696478354 ) ) ;
#3726 = CARTESIAN_POINT ( 'NONE',  ( 13.12018455494123081, 69.54296377198190271, -3.179949692328717159 ) ) ;
#3727 = CARTESIAN_POINT ( 'NONE',  ( 1.876532330890708260E-11, 6.313974596214807278, -12.00000000000000355 ) ) ;
#3728 = CARTESIAN_POINT ( 'NONE',  ( 11.84345469503521464, 30.18954924114118299, 6.489769361157302185 ) ) ;
#3729 = CARTESIAN_POINT ( 'NONE',  ( -11.52415037849118384, 55.66688209782287089, -7.052009664402310030 ) ) ;
#3730 = CARTESIAN_POINT ( 'NONE',  ( -12.01105834539781902, 50.16019076819019773, 6.249781159449053547 ) ) ;
#3731 = CARTESIAN_POINT ( 'NONE',  ( 3.705909840006434752, 64.04664249640974560, -12.98321921109010191 ) ) ;
#3732 = CARTESIAN_POINT ( 'NONE',  ( 10.34708690891700478, 42.76227428168909483, -8.671260026376653940 ) ) ;
#3733 = CARTESIAN_POINT ( 'NONE',  ( 13.48088785067486128, 39.39742276772284413, 0.9325739214256087983 ) ) ;
#3734 = ORIENTED_EDGE ( 'NONE', *, *, #16517, .T. ) ;
#3735 = CARTESIAN_POINT ( 'NONE',  ( 1.509281292405760415E-13, 1.813974596215571777, 12.00000000000000178 ) ) ;
#3736 = CARTESIAN_POINT ( 'NONE',  ( -7.781309575702445969, 70.47319914026155629, -11.03183906678731141 ) ) ;
#3737 = CARTESIAN_POINT ( 'NONE',  ( -4.127570232279888174, 61.32841266336937025, -12.85361106895534355 ) ) ;
#3738 = CARTESIAN_POINT ( 'NONE',  ( -3.636496289402152637, 3.329999999999999627, -11.19198476289190936 ) ) ;
#3739 = ORIENTED_EDGE ( 'NONE', *, *, #15969, .T. ) ;
#3740 = CARTESIAN_POINT ( 'NONE',  ( -5.847339916432642504, 40.39291978250835768, -12.16879597960247494 ) ) ;
#3741 = ORIENTED_EDGE ( 'NONE', *, *, #1418, .T. ) ;
#3742 = CARTESIAN_POINT ( 'NONE',  ( 13.50000000000000355, 24.58000000000001606, -4.386415899144233244 ) ) ;
#3743 = CARTESIAN_POINT ( 'NONE',  ( 13.16986379959834075, -64.51874999999984084, 13.16986379960055231 ) ) ;
#3744 = CARTESIAN_POINT ( 'NONE',  ( 1.121066298875345035, 61.13973486878198571, -13.46140389959024120 ) ) ;
#3745 = CIRCLE ( 'NONE', #4312, 22.50000000000000355 ) ;
#3746 = CARTESIAN_POINT ( 'NONE',  ( 12.46100838988894388, 57.24085334314524687, 5.193585410646714529 ) ) ;
#3747 = CARTESIAN_POINT ( 'NONE',  ( 7.272992578804311492, 79.87999999999999545, -10.01041549318726709 ) ) ;
#3748 = CARTESIAN_POINT ( 'NONE',  ( -13.49999999999999822, 36.78000000000000114, -4.386415899144240349 ) ) ;
#3749 = CARTESIAN_POINT ( 'NONE',  ( -11.76794919243112325, 81.07999999999998408, 3.823638476888994386 ) ) ;
#3750 = CARTESIAN_POINT ( 'NONE',  ( 10.92172942406179104, 1.730000000000009308, -7.935100905948385908 ) ) ;
#3751 = EDGE_CURVE ( 'NONE', #14160, #1419, #6919, .T. ) ;
#3752 = CARTESIAN_POINT ( 'NONE',  ( 5.348135253449231463, -100.0000000000000000, 12.08639588262338016 ) ) ;
#3753 = CARTESIAN_POINT ( 'NONE',  ( 25.42428528562856727, 0.000000000000000000, -5.441113646577394825 ) ) ;
#3754 = CARTESIAN_POINT ( 'NONE',  ( -8.043339635996302306, -6.243749999999984368, -8.043339635997654113 ) ) ;
#3755 =( BOUNDED_CURVE ( )  B_SPLINE_CURVE ( 2, ( #13951, #4781, #4694, #12645, #3176, #10099, #7261, #11587, #15275, #16963, #10014, #15362, #4865 ),
 .UNSPECIFIED., .F., .F. ) 
 B_SPLINE_CURVE_WITH_KNOTS ( ( 3, 2, 2, 2, 2, 2, 3 ),
 ( 0.2638888888888888951, 0.2666666666666666630, 0.2722222222222221988, 0.2777777777777777901, 0.2833333333333333259, 0.2888888888888888618, 0.2916666666666666297 ),
 .UNSPECIFIED. ) 
 CURVE ( )  GEOMETRIC_REPRESENTATION_ITEM ( )  RATIONAL_B_SPLINE_CURVE ( ( 0.9755282581475768211, 0.9755282581475768211, 1.000000000000000000, 0.9510565162951535312, 1.000000000000000000, 0.9510565162951535312, 1.000000000000000000, 0.9510565162951535312, 1.000000000000000000, 0.9510565162951535312, 1.000000000000000000, 0.9755282581475770431, 0.9755282581475768211 ) ) 
 REPRESENTATION_ITEM ( '' )  );
#3756 = AXIS2_PLACEMENT_3D ( 'NONE', #10322, #15769, #678 ) ;
#3757 = CARTESIAN_POINT ( 'NONE',  ( 8.343458848123583849, 44.87999999999998835, -11.48378591275253768 ) ) ;
#3758 = CARTESIAN_POINT ( 'NONE',  ( 2.435307549839813124, 34.09246322853890376, -13.28282044714515031 ) ) ;
#3759 = CARTESIAN_POINT ( 'NONE',  ( -7.465912594396658442, 73.45946290405333912, -11.24767626733296133 ) ) ;
#3760 = VERTEX_POINT ( 'NONE', #6739 ) ;
#3761 = VERTEX_POINT ( 'NONE', #6827 ) ;
#3762 = CARTESIAN_POINT ( 'NONE',  ( -7.272992578804310604, 75.37999999999999545, 10.01041549318726886 ) ) ;
#3763 = ORIENTED_EDGE ( 'NONE', *, *, #15079, .F. ) ;
#3764 = CARTESIAN_POINT ( 'NONE',  ( -4.171729424061791036, 17.53000000000001890, 12.83926296998457239 ) ) ;
#3765 = CARTESIAN_POINT ( 'NONE',  ( 11.37499999999999645, -57.19999999999988916, 9.531744055041752924E-13 ) ) ;
#3766 = CARTESIAN_POINT ( 'NONE',  ( -7.682391541889500353, 44.39115312923465950, 11.10122368241315449 ) ) ;
#3767 = CARTESIAN_POINT ( 'NONE',  ( -7.499999999999994671, -27.00452558693060467, -5.560661329642323736 ) ) ;
#3768 = CARTESIAN_POINT ( 'NONE',  ( 12.53368164500171389, 66.61264531847000114, -5.027186995046044160 ) ) ;
#3769 = CARTESIAN_POINT ( 'NONE',  ( -13.50000000000000000, 49.92999999999999972, -3.306546357697853733E-15 ) ) ;
#3770 = CARTESIAN_POINT ( 'NONE',  ( -3.162095574282764776, 71.56630276718368577, 13.12444876022228435 ) ) ;
#3771 = EDGE_CURVE ( 'NONE', #5443, #4554, #9793, .T. ) ;
#3772 = CARTESIAN_POINT ( 'NONE',  ( 13.16986379960055054, -68.68124999999983515, -13.16986379959834430 ) ) ;
#3773 = CARTESIAN_POINT ( 'NONE',  ( -13.32309267394441221, 68.00683485648823989, 2.188465561525937186 ) ) ;
#3774 = CARTESIAN_POINT ( 'NONE',  ( 18.62500000000000000, -83.24999999999980105, 1.560692158462880521E-12 ) ) ;
#3775 = CARTESIAN_POINT ( 'NONE',  ( 4.857942641284302532, 55.00488871956680725, -12.59565032908122006 ) ) ;
#3776 = CARTESIAN_POINT ( 'NONE',  ( 3.636496289402157078, 21.02999999999999403, -11.19198476289190936 ) ) ;
#3777 = CARTESIAN_POINT ( 'NONE',  ( -1.564113515457998572E-12, -62.43749999999985079, 18.62500000000000000 ) ) ;
#3778 = DIRECTION ( 'NONE',  ( 0.8660254037844400399, 0.000000000000000000, -0.4999999999999976685 ) ) ;
#3779 = CARTESIAN_POINT ( 'NONE',  ( -1.104890279304959755, 62.64030871745742957, 13.46071023764019259 ) ) ;
#3780 = CARTESIAN_POINT ( 'NONE',  ( -9.362710248175982741, 35.31320775059099049, 9.725773573732148236 ) ) ;
#3781 = VERTEX_POINT ( 'NONE', #3898 ) ;
#3782 = DIRECTION ( 'NONE',  ( 0.000000000000000000, 0.000000000000000000, 1.000000000000000000 ) ) ;
#3783 = CARTESIAN_POINT ( 'NONE',  ( -13.49475676771158383, 31.91478873253841186, -0.4353569615216364985 ) ) ;
#3784 = B_SPLINE_CURVE_WITH_KNOTS ( 'NONE', 3,
 ( #10054, #12863, #15404, #2060, #6240, #3311, #10306, #8725, #3401, #14339, #2315, #6072, #15575, #2228, #16829, #9074, #15751, #7743, #14083, #14254, #8813, #1970, #12775, #663, #7568, #917, #15490, #7482 ),
 .UNSPECIFIED., .F., .F.,
 ( 4, 2, 2, 2, 2, 2, 2, 2, 2, 2, 2, 2, 2, 4 ),
 ( 1.666147490140627990E-16, 0.002883762942657031644, 0.004325644413985462247, 0.005767525885313893284, 0.008651288827970756226, 0.01009317029929918813, 0.01153505177062761830, 0.01297693324195605021, 0.01441881471328448211, 0.01730257765594134592, 0.01874445912726978303, 0.02018634059859821667, 0.02162822206992665031, 0.02307010354125508395 ),
 .UNSPECIFIED. ) ;
#3785 = DIRECTION ( 'NONE',  ( -0.000000000000000000, -0.000000000000000000, 1.000000000000000000 ) ) ;
#3786 = CARTESIAN_POINT ( 'NONE',  ( 9.203170713077465592, 60.03895907460095316, 9.877926015694953321 ) ) ;
#3787 = CARTESIAN_POINT ( 'NONE',  ( -13.50000000000000000, -3.069999999999996287, -3.469446951953614189E-15 ) ) ;
#3788 = CARTESIAN_POINT ( 'NONE',  ( -9.925890167077604076, 53.28464950770988651, 9.150231210120352898 ) ) ;
#3789 = CARTESIAN_POINT ( 'NONE',  ( -11.76794919243112325, 53.92999999999999972, -2.882316262207890869E-15 ) ) ;
#3790 = SHAPE_DEFINITION_REPRESENTATION ( #6933, #5468 ) ;
#3791 = CARTESIAN_POINT ( 'NONE',  ( 5.363543519840087370, 50.87413298173109411, 12.39218804481266645 ) ) ;
#3792 = CARTESIAN_POINT ( 'NONE',  ( -13.47203084398158524, 37.90000543725030724, -0.8690430185918386341 ) ) ;
#3793 = AXIS2_PLACEMENT_3D ( 'NONE', #13494, #5473, #14805 ) ;
#3794 = CARTESIAN_POINT ( 'NONE',  ( 11.73271526642915141, 36.67822783863627478, -6.684209631556711884 ) ) ;
#3795 = CARTESIAN_POINT ( 'NONE',  ( -4.711679271993001628, -45.75312499999991189, -11.37500000000039613 ) ) ;
#3796 = CARTESIAN_POINT ( 'NONE',  ( -0.7060178253421292016, 74.65461446910167354, 13.48159923038322638 ) ) ;
#3797 = PRODUCT_DEFINITION_SHAPE ( 'NONE', 'NONE',  #3168 ) ;
#3798 = CARTESIAN_POINT ( 'NONE',  ( -12.64011703651372187, 77.10247514769642407, 4.761869442916747630 ) ) ;
#3799 = CARTESIAN_POINT ( 'NONE',  ( -13.32733280186987024, 80.00689698629075508, 2.196482157303579985 ) ) ;
#3800 = DIRECTION ( 'NONE',  ( 1.000000000000000000, 0.000000000000000000, 0.000000000000000000 ) ) ;
#3801 = VERTEX_POINT ( 'NONE', #1590 ) ;
#3802 = CARTESIAN_POINT ( 'NONE',  ( 0.000000000000000000, 9.000000000000000000, 0.000000000000000000 ) ) ;
#3803 = CARTESIAN_POINT ( 'NONE',  ( 3.636496289402157078, 15.03000000000001535, -11.19198476289190936 ) ) ;
#3804 = ORIENTED_EDGE ( 'NONE', *, *, #7234, .T. ) ;
#3805 = CARTESIAN_POINT ( 'NONE',  ( -9.520470885617717371, 54.23000000000000398, 6.917026985038133624 ) ) ;
#3806 = CARTESIAN_POINT ( 'NONE',  ( 11.37500000000000000, 4.439344646909156023E-16, 9.531744055041752924E-13 ) ) ;
#3807 = FACE_OUTER_BOUND ( 'NONE', #12680, .T. ) ;
#3808 = CARTESIAN_POINT ( 'NONE',  ( -4.171729424061787483, -7.669999999999996376, -12.83926296998457417 ) ) ;
#3809 = CARTESIAN_POINT ( 'NONE',  ( 6.186989602441420821, 75.95361305086539971, -11.99880612961145587 ) ) ;
#3810 = DIRECTION ( 'NONE',  ( 0.000000000000000000, 0.000000000000000000, -1.000000000000000000 ) ) ;
#3811 = CARTESIAN_POINT ( 'NONE',  ( 10.92172942406178926, 72.12999999999999545, 7.935100905948387684 ) ) ;
#3812 = CARTESIAN_POINT ( 'NONE',  ( 7.272992578804311492, 43.87999999999999545, -10.01041549318726709 ) ) ;
#3813 = DIRECTION ( 'NONE',  ( 2.806191565803427284E-15, 0.000000000000000000, -1.000000000000000000 ) ) ;
#3814 = CARTESIAN_POINT ( 'NONE',  ( -11.53975138069232109, 58.66770748737323515, -7.033342735042283245 ) ) ;
#3815 = CARTESIAN_POINT ( 'NONE',  ( 7.168473922838755286, 44.94694224986446329, 11.44171851688767916 ) ) ;
#3816 = CARTESIAN_POINT ( 'NONE',  ( 11.08577043759925118, 69.72028810587863745, -7.704379851462255679 ) ) ;
#3817 = CARTESIAN_POINT ( 'NONE',  ( -10.92172942406178926, 66.62999999999999545, -7.935100905948389460 ) ) ;
#3818 = CARTESIAN_POINT ( 'NONE',  ( -9.708203932499367639, 3.763974596215556190, -7.053423027509681198 ) ) ;
#3819 = CARTESIAN_POINT ( 'NONE',  ( -1.977116238977308482, 55.25103791471835279, -13.36401229022775361 ) ) ;
#3820 = CARTESIAN_POINT ( 'NONE',  ( -5.519339117068075673, 50.47982862213257249, 12.32018707268373703 ) ) ;
#3821 = CARTESIAN_POINT ( 'NONE',  ( 9.703181444203755390, 63.79612580964563762, -9.386421454467969383 ) ) ;
#3822 = CARTESIAN_POINT ( 'NONE',  ( 11.92514546446363788, 42.66388649755253226, -6.327788414984513388 ) ) ;
#3823 = CARTESIAN_POINT ( 'NONE',  ( 12.51531601377990022, 39.24597988571901652, 5.061315126527163422 ) ) ;
#3824 = ORIENTED_EDGE ( 'NONE', *, *, #4756, .T. ) ;
#3825 = CARTESIAN_POINT ( 'NONE',  ( -13.39686745019108294, 70.87189925962454140, -1.665516949025961368 ) ) ;
#3826 = CARTESIAN_POINT ( 'NONE',  ( -12.18511954038002365, 61.71674294599442590, -5.811709024524145839 ) ) ;
#3827 = CARTESIAN_POINT ( 'NONE',  ( 9.520470885617717371, 8.730000000000014637, -6.917026985038131848 ) ) ;
#3828 = VERTEX_POINT ( 'NONE', #9316 ) ;
#3829 = ORIENTED_EDGE ( 'NONE', *, *, #8420, .F. ) ;
#3830 = CARTESIAN_POINT ( 'NONE',  ( 8.343458848123578520, 23.98000000000000753, 11.48378591275254124 ) ) ;
#3831 = CARTESIAN_POINT ( 'NONE',  ( 1.561832610794586538E-12, -70.76249999999983231, -18.62500000000000000 ) ) ;
#3832 = EDGE_CURVE ( 'NONE', #7801, #17099, #5504, .T. ) ;
#3833 = CARTESIAN_POINT ( 'NONE',  ( 3.086401082262576256, 61.06902437418678176, -13.14245697113578437 ) ) ;
#3834 = VECTOR ( 'NONE', #14029, 1000.000000000000000 ) ;
#3835 = CARTESIAN_POINT ( 'NONE',  ( 12.35346123165463617, 57.62892738134787862, -5.444651084883814995 ) ) ;
#3836 = CARTESIAN_POINT ( 'NONE',  ( 3.636496289402157078, 68.03000000000000114, -11.19198476289190936 ) ) ;
#3837 = CARTESIAN_POINT ( 'NONE',  ( 11.76794919243112680, 76.57999999999998408, -3.823638476888993942 ) ) ;
#3838 = CARTESIAN_POINT ( 'NONE',  ( -0.5808156989666466430, 47.65911991592597730, 13.48844809475130369 ) ) ;
#3839 = CARTESIAN_POINT ( 'NONE',  ( 4.711679271993006068, -30.17812499999993747, 11.37500000000039257 ) ) ;
#3840 = COLOUR_RGB ( '',0.7921568627450980005, 0.8196078431372548767, 0.9333333333333333481 ) ;
#3841 = PLANE ( 'NONE',  #10916 ) ;
#3842 = CYLINDRICAL_SURFACE ( 'NONE', #3364, 13.50000000000000000 ) ;
#3843 = CARTESIAN_POINT ( 'NONE',  ( -5.073760196756867735, 73.36319280854625902, -12.51029294622204446 ) ) ;
#3844 = ORIENTED_EDGE ( 'NONE', *, *, #4416, .F. ) ;
#3845 = ORIENTED_EDGE ( 'NONE', *, *, #75, .F. ) ;
#3846 = CARTESIAN_POINT ( 'NONE',  ( -11.76794919243112325, 77.92999999999999261, -2.882316262207890869E-15 ) ) ;
#3847 = ORIENTED_EDGE ( 'NONE', *, *, #7267, .T. ) ;
#3848 = CARTESIAN_POINT ( 'NONE',  ( -11.37499999999960210, -64.48437499999987210, -4.711679271994911211 ) ) ;
#3849 = CARTESIAN_POINT ( 'NONE',  ( -0.5815368319779855577, 44.65908970977663017, 13.48758275782939542 ) ) ;
#3850 = EDGE_CURVE ( 'NONE', #9365, #9933, #4414, .T. ) ;
#3851 = CARTESIAN_POINT ( 'NONE',  ( -7.499999999999995559, -27.55009420329275827, 3.560038493048078845 ) ) ;
#3852 = CARTESIAN_POINT ( 'NONE',  ( 13.39960944229175333, 66.48731185255626031, -1.643332913497620451 ) ) ;
#3853 = AXIS2_PLACEMENT_3D ( 'NONE', #11306, #15346, #3247 ) ;
#3854 = CARTESIAN_POINT ( 'NONE',  ( -8.691771469529815392E-16, 44.67999999999999972, 14.19474002721660355 ) ) ;
#3855 = CARTESIAN_POINT ( 'NONE',  ( -8.293551300264768500, 71.36388038614214224, 10.65233661047543556 ) ) ;
#3856 = CARTESIAN_POINT ( 'NONE',  ( -18.62500000000064659, -59.31562499999985505, 7.714727599197335195 ) ) ;
#3857 = CARTESIAN_POINT ( 'NONE',  ( -13.42158662539458192, 67.87941032537437991, -1.453869035909064467 ) ) ;
#3858 = CARTESIAN_POINT ( 'NONE',  ( -18.62500000000000000, -1.074999999999978639, -1.562973063126292757E-12 ) ) ;
#3859 = CARTESIAN_POINT ( 'NONE',  ( 7.145042507201743831, 54.91449063741976744, -11.46286542413573173 ) ) ;
#3860 = CARTESIAN_POINT ( 'NONE',  ( -11.76794919243112325, 18.78000000000001180, -3.823638476888998827 ) ) ;
#3861 = CARTESIAN_POINT ( 'NONE',  ( -7.714727599200467800, -78.04687499999982947, 18.62499999999934630 ) ) ;
#3862 = CARTESIAN_POINT ( 'NONE',  ( -12.77386615626469535, 65.08747835186800046, 4.369140299076793355 ) ) ;
#3863 = CARTESIAN_POINT ( 'NONE',  ( -5.432056264447402860, 35.48329878629467515, 12.36543368378323748 ) ) ;
#3864 = ORIENTED_EDGE ( 'NONE', *, *, #10758, .T. ) ;
#3865 = CARTESIAN_POINT ( 'NONE',  ( 9.335235950531815854E-15, 8.180000000000005045, -13.50000000000000178 ) ) ;
#3866 = EDGE_CURVE ( 'NONE', #13443, #743, #9296, .T. ) ;
#3867 = CARTESIAN_POINT ( 'NONE',  ( 2.279995255611139653E-15, 27.18000000000000682, -12.37355403259654985 ) ) ;
#3868 = CARTESIAN_POINT ( 'NONE',  ( -3.785303478180469305, 31.31610501778620659, -12.96062533801228689 ) ) ;
#3869 = DIRECTION ( 'NONE',  ( 0.000000000000000000, -1.000000000000000000, 0.000000000000000000 ) ) ;
#3870 = CARTESIAN_POINT ( 'NONE',  ( 12.93954261948424111, 60.29192777250819546, 3.855782101392678740 ) ) ;
#3871 = CARTESIAN_POINT ( 'NONE',  ( -8.374943186797883854, 53.36072342052383988, 10.60918593187694192 ) ) ;
#3872 = CARTESIAN_POINT ( 'NONE',  ( 11.76794919243112680, 46.57999999999999829, -3.823638476888993942 ) ) ;
#3873 = PRODUCT_CONTEXT ( 'NONE', #17138, 'mechanical' ) ;
#3874 = CARTESIAN_POINT ( 'NONE',  ( -13.49999999999999822, 69.78000000000000114, -4.386415899144240349 ) ) ;
#3875 = CARTESIAN_POINT ( 'NONE',  ( 8.243599928797097576, 50.99384897302891062, 10.69102843549329940 ) ) ;
#3876 = CARTESIAN_POINT ( 'NONE',  ( -11.88435525982994889, 37.69305171285699174, -6.404073035000328318 ) ) ;
#3877 = CARTESIAN_POINT ( 'NONE',  ( 10.51734625305970461, 36.10681963769080483, 8.466829602298034274 ) ) ;
#3878 = CARTESIAN_POINT ( 'NONE',  ( -11.37500000000039613, -99.86562499999978115, 4.711679271993000739 ) ) ;
#3879 = CARTESIAN_POINT ( 'NONE',  ( -6.050054063620305733, 74.45907014989788308, 12.06844880531143360 ) ) ;
#3880 = CARTESIAN_POINT ( 'NONE',  ( -13.50069008547208860, 76.92950476662907988, -0.01155620547472042438 ) ) ;
#3881 = CARTESIAN_POINT ( 'NONE',  ( -10.15564728739121669, 80.27272457646746773, 8.905508388590966717 ) ) ;
#3882 = CARTESIAN_POINT ( 'NONE',  ( 9.520470885617715595, 11.13000000000000078, 6.917026985038135400 ) ) ;
#3883 = CARTESIAN_POINT ( 'NONE',  ( 7.500000000000001776, 105.3920397463311218, 8.709571264514705646 ) ) ;
#3884 = CARTESIAN_POINT ( 'NONE',  ( -7.499999999999998224, 108.9300000000000068, -9.367496997597600128 ) ) ;
#3885 = CARTESIAN_POINT ( 'NONE',  ( 7.272992578804308828, 4.980000000000008420, 10.01041549318726709 ) ) ;
#3886 = CARTESIAN_POINT ( 'NONE',  ( 9.520470885617717371, 52.72999999999999687, -6.917026985038131848 ) ) ;
#3887 = CARTESIAN_POINT ( 'NONE',  ( 8.043339635996302306, -40.61874999999988489, 8.043339635997654113 ) ) ;
#3888 = CARTESIAN_POINT ( 'NONE',  ( -13.16986379959834252, -6.243749999999985256, -13.16986379960055054 ) ) ;
#3889 = CARTESIAN_POINT ( 'NONE',  ( -13.50000000000000000, -10.06999999999999496, -3.469446951953614189E-15 ) ) ;
#3890 = PLANE ( 'NONE',  #4324 ) ;
#3891 = CARTESIAN_POINT ( 'NONE',  ( 3.905267433998111493, 76.03955353119496863, -12.92325076002208206 ) ) ;
#3892 = CARTESIAN_POINT ( 'NONE',  ( 18.62500000000000000, -99.89999999999976410, 0.000000000000000000 ) ) ;
#3893 = CARTESIAN_POINT ( 'NONE',  ( -11.76794919243112325, 38.77999999999999403, -3.823638476888998827 ) ) ;
#3894 = DIRECTION ( 'NONE',  ( -1.000000000000000000, -8.673617379884037937E-17, 0.000000000000000000 ) ) ;
#3895 = CARTESIAN_POINT ( 'NONE',  ( -13.14170631426251212, 58.81803730528373819, -3.156520166358864010 ) ) ;
#3896 = CARTESIAN_POINT ( 'NONE',  ( 2.884611534850368475, 44.78371962230355052, 13.18822724452614459 ) ) ;
#3897 = CARTESIAN_POINT ( 'NONE',  ( 12.37795243579363635, 69.62700217947723047, -5.400564600271921201 ) ) ;
#3898 = CARTESIAN_POINT ( 'NONE',  ( 2.445080149700053643E-15, 33.17999999999999261, -13.50000000000000000 ) ) ;
#3899 = CARTESIAN_POINT ( 'NONE',  ( 8.719434965209991617, 30.01580748498589202, 10.30804611199927301 ) ) ;
#3900 = EDGE_CURVE ( 'NONE', #3211, #16090, #6391, .T. ) ;
#3901 = CARTESIAN_POINT ( 'NONE',  ( -10.11073118668884874, 55.58505174064411136, -8.945568110028689901 ) ) ;
#3902 = CARTESIAN_POINT ( 'NONE',  ( -5.538802633866588110, 50.47907763144620930, 12.31144910959687877 ) ) ;
#3903 = CARTESIAN_POINT ( 'NONE',  ( 11.51750660560541561, 63.69287151518827983, -7.042528692690322778 ) ) ;
#3904 = CARTESIAN_POINT ( 'NONE',  ( 13.05580366346349841, 42.55242448848036929, -3.435679632562075980 ) ) ;
#3905 = CARTESIAN_POINT ( 'NONE',  ( 9.165837416579254437, 39.03714869363280116, 9.911684281184246714 ) ) ;
#3906 = CIRCLE ( 'NONE', #10419, 12.00000000000000178 ) ;
#3907 = ORIENTED_EDGE ( 'NONE', *, *, #15057, .T. ) ;
#3908 = CARTESIAN_POINT ( 'NONE',  ( -9.881012300872606957, 70.57302064171045686, -9.198673637768660427 ) ) ;
#3909 = DIRECTION ( 'NONE',  ( -0.000000000000000000, 1.000000000000000000, -0.000000000000000000 ) ) ;
#3910 = CARTESIAN_POINT ( 'NONE',  ( 9.520470885617717371, 2.730000000000010196, -6.917026985038131848 ) ) ;
#3911 = ORIENTED_EDGE ( 'NONE', *, *, #8030, .F. ) ;
#3912 = EDGE_LOOP ( 'NONE', ( #10047, #1056, #6154, #6746 ) ) ;
#3913 = CARTESIAN_POINT ( 'NONE',  ( -13.50000000000000000, 19.93000000000000327, -3.469446951953614189E-15 ) ) ;
#3914 = CARTESIAN_POINT ( 'NONE',  ( -1.564113515457998572E-12, -95.73749999999976978, 18.62500000000000000 ) ) ;
#3915 = CARTESIAN_POINT ( 'NONE',  ( -1.005545769327274827E-13, 52.18000000000000682, -13.50000000000000000 ) ) ;
#3916 = CARTESIAN_POINT ( 'NONE',  ( 13.50000000000000355, 10.57999999999999119, -4.386415899144233244 ) ) ;
#3917 = CARTESIAN_POINT ( 'NONE',  ( 8.310874194162975570, 71.99679895926327333, 10.64270930270453341 ) ) ;
#3918 = CARTESIAN_POINT ( 'NONE',  ( 13.06949918658192367, 57.55469024356798258, -3.496992391659727417 ) ) ;
#3919 = CARTESIAN_POINT ( 'NONE',  ( -7.272992578804307939, 65.48000000000000398, -10.01041549318726886 ) ) ;
#3920 = CARTESIAN_POINT ( 'NONE',  ( 7.272992578804311492, 76.88000000000000966, -10.01041549318726709 ) ) ;
#3921 = CARTESIAN_POINT ( 'NONE',  ( -11.42340091696314630, 47.19916785071956156, 7.194499597321170725 ) ) ;
#3922 = CIRCLE ( 'NONE', #8466, 9.000000000000000000 ) ;
#3923 = LINE ( 'NONE', #6941, #16031 ) ;
#3924 = DIRECTION ( 'NONE',  ( -0.000000000000000000, 1.000000000000000000, -0.000000000000000000 ) ) ;
#3925 = CARTESIAN_POINT ( 'NONE',  ( -3.998255974501887078, 10.00000000000000888, -12.30404106125027575 ) ) ;
#3926 = CARTESIAN_POINT ( 'NONE',  ( 4.711679271994911211, -79.12187499999980389, -11.37499999999960743 ) ) ;
#3927 = DIRECTION ( 'NONE',  ( 0.000000000000000000, -1.000000000000000000, 0.000000000000000000 ) ) ;
#3928 = CARTESIAN_POINT ( 'NONE',  ( 11.99720772546109693, 33.65837649682584498, -6.190075193952552901 ) ) ;
#3929 = CARTESIAN_POINT ( 'NONE',  ( -7.006031218443153463, 73.43963910418750629, -11.55271937892839063 ) ) ;
#3930 = ORIENTED_EDGE ( 'NONE', *, *, #6778, .F. ) ;
#3931 = ORIENTED_EDGE ( 'NONE', *, *, #12689, .F. ) ;
#3932 = CARTESIAN_POINT ( 'NONE',  ( -3.636496289402153081, 77.32999999999999829, -11.19198476289190936 ) ) ;
#3933 = VERTEX_POINT ( 'NONE', #9841 ) ;
#3934 = CARTESIAN_POINT ( 'NONE',  ( -13.31322428518614309, 41.00862424342748369, 2.238198738180153136 ) ) ;
#3935 = CARTESIAN_POINT ( 'NONE',  ( 8.043339635996298753, -55.11874999999988489, 8.043339635997652337 ) ) ;
#3936 = VECTOR ( 'NONE', #12887, 1000.000000000000000 ) ;
#3937 = CARTESIAN_POINT ( 'NONE',  ( -10.19438961638010177, 44.27054227623447247, 8.850209172380360201 ) ) ;
#3938 = CARTESIAN_POINT ( 'NONE',  ( -7.499999999999993783, -26.56718630404941806, -6.484415072061725738 ) ) ;
#3939 = PRODUCT_DEFINITION ( 'UNKNOWN', '', #6528, #10736 ) ;
#3940 = CARTESIAN_POINT ( 'NONE',  ( -10.92172942406179104, 41.22999999999999687, 7.935100905948387684 ) ) ;
#3941 = CARTESIAN_POINT ( 'NONE',  ( -6.957400787806288456, 71.42232733259757538, 11.58147395634350296 ) ) ;
#3942 = CARTESIAN_POINT ( 'NONE',  ( 7.714727599200456254, -12.52187499999995524, -18.62499999999935341 ) ) ;
#3943 = CARTESIAN_POINT ( 'NONE',  ( -12.92540607541860886, 68.06966242483530038, 3.897284986388191097 ) ) ;
#3944 = CARTESIAN_POINT ( 'NONE',  ( -18.62500000000064659, -92.61562499999978115, 7.714727599197335195 ) ) ;
#3945 = EDGE_CURVE ( 'NONE', #8869, #3432, #3087, .T. ) ;
#3946 = CARTESIAN_POINT ( 'NONE',  ( 10.46984184081570568, 54.75555934975864858, -8.522531150578997128 ) ) ;
#3947 = CARTESIAN_POINT ( 'NONE',  ( -3.636496289402152637, 21.33000000000001606, -11.19198476289190936 ) ) ;
#3948 = CARTESIAN_POINT ( 'NONE',  ( 18.62500000000000000, -99.89999999999976410, 1.560692158462880521E-12 ) ) ;
#3949 = CARTESIAN_POINT ( 'NONE',  ( -13.39894528404028406, 64.87027492873734502, -1.716493634713462724 ) ) ;
#3950 = B_SPLINE_CURVE_WITH_KNOTS ( 'NONE', 3,
 ( #15374, #11512, #3541, #7456, #4620, #10026, #14057, #8955, #886, #1944, #723, #12836, #6132, #12919, #7626, #16887, #4794, #10195, #2112, #14313, #2199, #6298, #10621, #15813, #14573, #3891, #10455, #7806, #16073, #12111, #8065, #1151, #6563, #13428, #3809, #9308, #3718, #1, #15900, #11943, #15721, #15987, #9222, #11770, #14659, #13090, #2547, #13177, #9135, #6475, #7712, #1235, #14395, #2457, #6732, #14484, #7976, #3627, #7887, #17237, #2371, #12028, #1063, #6387, #11861, #6647, #1317, #5147, #17323, #13345, #10538, #2284, #13264, #3980, #5235, #17407, #17147, #5056, #975, #5322, #10706, #9394, #14744, #2634, #10368, #9043, #6912, #1670, #2986, #9567, #16519, #1759, #8242, #15087, #8417, #9655, #8506, #12376, #12555, #5759, #15179, #5677, #4245, #92, #12288, #8329, #9834, #269, #11057, #10878, #15006, #16430, #5497, #2810, #11143, #7169, #3079, #13684, #1582, #13855, #16338, #7084, #2897, #5407, #13768, #4333, #12468, #9742, #10969, #6822, #353, #8150, #4425, #13602, #4155, #1497, #2722, #10792, #9482, #7000, #16157, #4066, #14828, #14917, #13514, #1406, #12200, #16249, #182, #5590, #15354, #8853, #8933, #526, #2009, #702, #1925, #4512, #14037, #6192, #4688, #7603, #10007, #16867, #9919, #8592, #16954, #11316, #15527, #7346, #14207, #14292, #12727, #2091, #3437, #4600, #11579, #2177, #3258, #10177, #7518, #16693, #12898, #785, #10091, #16779, #16607, #613, #6112, #441, #6024, #5850, #4856, #13943, #8678, #7435, #10259, #15269, #11232, #3166, #12814, #11408, #15611, #15442 ),
 .UNSPECIFIED., .F., .F.,
 ( 4, 2, 2, 2, 2, 1, 1, 1, 2, 2, 2, 2, 2, 1, 1, 1, 2, 2, 2, 2, 2, 2, 2, 2, 2, 2, 1, 1, 1, 2, 2, 1, 2, 2, 1, 2, 2, 1, 2, 2, 2, 2, 1, 2, 2, 2, 2, 2, 2, 2, 2, 1, 1, 1, 2, 2, 2, 1, 1, 1, 2, 2, 2, 2, 2, 2, 2, 2, 1, 1, 2, 2, 2, 2, 1, 2, 2, 2, 2, 2, 1, 1, 2, 2, 2, 1, 2, 2, 2, 2, 2, 2, 2, 2, 2, 2, 1, 2, 2, 2, 2, 2, 2, 1, 1, 1, 1, 2, 2, 2, 1, 2, 2, 1, 1, 1, 2, 2, 4 ),
 ( 0.09315741062983846910, 0.09361976615167078020, 0.09373535503212884756, 0.09374980364218611639, 0.09375702794721474387, 0.09376425225224337134, 0.09379314947235789512, 0.09385094391258694269, 0.09408212167350313293, 0.09500683271716785228, 0.09546918823900021889, 0.09570036599991640913, 0.09571481460997366408, 0.09572926322003093291, 0.09575816044014544282, 0.09581595488037449038, 0.09593154376083258550, 0.09685625480449729097, 0.09731861032632964370, 0.09754978808724582007, 0.09760758252747486763, 0.09766537696770391519, 0.09778096584816199643, 0.09870567689182659088, 0.09916803241365888810, 0.09939921017457503671, 0.09951479905503310408, 0.09957259349526213776, 0.09960149071537666154, 0.09960871502040528902, 0.09961593932543391650, 0.09963038793549117145, 0.1005550989791556965, 0.1014798100228202216, 0.1015376044630492552, 0.1015520530731065102, 0.1015665016831637651, 0.1015953989032782889, 0.1017109877837363424, 0.1019421655446524494, 0.1024045210664846772, 0.1033292321101491468, 0.1034448209906072003, 0.1035026154308362339, 0.1035604098710652538, 0.1037915876319813885, 0.1042539431538136718, 0.1051786541974782246, 0.1054098319583943594, 0.1054676263986233931, 0.1054748507036520205, 0.1054820750086806480, 0.1054965236187379168, 0.1055254208388524267, 0.1056410097193104802, 0.1061033652411427081, 0.1070280762848071499, 0.1072592540457232568, 0.1073748429261813103, 0.1074037401462958341, 0.1074181887563530891, 0.1074326373664103440, 0.1074904318066393638, 0.1079527873284715639, 0.1088774983721359502, 0.1093398538939681364, 0.1093687511140826463, 0.1093976483341971701, 0.1094554427744262037, 0.1095710316548842572, 0.1098022094158003781, 0.1116516315031293033, 0.1118828092640454241, 0.1119406037042744440, 0.1119983981445034776, 0.1121139870249615311, 0.1125763425467937590, 0.1130386980686259868, 0.1131542869490840403, 0.1132120813893130601, 0.1132698758295420938, 0.1135010535904582007, 0.1144257646341226564, 0.1144546618542371802, 0.1144835590743516901, 0.1145413535145807377, 0.1146569423950388467, 0.1148881201559550369, 0.1153504756777874452, 0.1162751867214522616, 0.1163329811616813092, 0.1163907756019103706, 0.1165063644823684796, 0.1167375422432846838, 0.1171998977651171059, 0.1181246088087819501, 0.1182401976892400591, 0.1182979921294691067, 0.1183557865696981681, 0.1185869643306143723, 0.1190493198524467944, 0.1199740308961116525, 0.1199884795061689213, 0.1200029281162261763, 0.1200318253363407139, 0.1200896197765697615, 0.1202052086570278844, 0.1204363864179441301, 0.1208987419397766078, 0.1213610974616090854, 0.1215922752225253312, 0.1216500696627543926, 0.1216572939677830201, 0.1216645182728116614, 0.1216789668828689303, 0.1217078641029834679, 0.1218234529834416047, 0.1222858085052741794, 0.1227481640271067542 ),
 .UNSPECIFIED. ) ;
#3951 = CARTESIAN_POINT ( 'NONE',  ( -9.257384347542936709, 35.31844601351780710, 9.826854653260157946 ) ) ;
#3952 = ORIENTED_EDGE ( 'NONE', *, *, #13794, .T. ) ;
#3953 = CARTESIAN_POINT ( 'NONE',  ( -2.707340708274796892, 3.720968205702271315E-15, -11.97265601701247384 ) ) ;
#3954 = CARTESIAN_POINT ( 'NONE',  ( -9.610466609222978462, 31.55914188783036423, -9.486719919042664984 ) ) ;
#3955 = CARTESIAN_POINT ( 'NONE',  ( 12.50000000000000000, -22.00000000000000355, -1.714505518806294835E-15 ) ) ;
#3956 = CARTESIAN_POINT ( 'NONE',  ( 11.76794919243112325, -12.56999999999999851, 1.734723475976807094E-15 ) ) ;
#3957 = CARTESIAN_POINT ( 'NONE',  ( -12.50000000000000000, -18.00000000000000355, -2.204364238465235822E-15 ) ) ;
#3958 = CARTESIAN_POINT ( 'NONE',  ( -10.92172942406178926, -3.369999999999997886, -7.935100905948389460 ) ) ;
#3959 =( BOUNDED_CURVE ( )  B_SPLINE_CURVE ( 2, ( #5783, #377, #11168, #11616, #6151 ),
 .UNSPECIFIED., .F., .F. ) 
 B_SPLINE_CURVE_WITH_KNOTS ( ( 3, 2, 3 ),
 ( 0.2424487531369445559, 0.2462071549303284645, 0.2503072064569185073 ),
 .UNSPECIFIED. ) 
 CURVE ( )  GEOMETRIC_REPRESENTATION_ITEM ( )  RATIONAL_B_SPLINE_CURVE ( ( 0.9755282581475768211, 0.9755282581474007397, 1.000000000000000000, 0.9733037051233607295, 0.9757304765342935671 ) ) 
 REPRESENTATION_ITEM ( '' )  );
#3960 = CARTESIAN_POINT ( 'NONE',  ( -9.845067486581010385, 53.28885231408968082, 9.237281070633853730 ) ) ;
#3961 = CARTESIAN_POINT ( 'NONE',  ( 3.636496289402154414, 48.82999999999999829, 11.19198476289190936 ) ) ;
#3962 = APPLICATION_PROTOCOL_DEFINITION ( 'draft international standard', 'automotive_design', 1998, #8130 ) ;
#3963 = CARTESIAN_POINT ( 'NONE',  ( 13.50000000000000355, 68.57999999999998408, -4.386415899144233244 ) ) ;
#3964 = CARTESIAN_POINT ( 'NONE',  ( 10.03500853364407064, 51.08076950763429380, 9.041007138082409966 ) ) ;
#3965 = CARTESIAN_POINT ( 'NONE',  ( -10.23891164854874702, 37.59188044157124864, -8.798564376260818776 ) ) ;
#3966 = EDGE_CURVE ( 'NONE', #10490, #7293, #4519, .T. ) ;
#3967 = CARTESIAN_POINT ( 'NONE',  ( 10.97156431219244510, 36.13285426820748114, 7.867357652818380842 ) ) ;
#3968 = CARTESIAN_POINT ( 'NONE',  ( -18.62499999999935341, -14.53437499999998650, -7.714727599200458030 ) ) ;
#3969 = CARTESIAN_POINT ( 'NONE',  ( -0.9212313319806377798, 74.64687916296506387, 13.46868817401126606 ) ) ;
#3970 = CARTESIAN_POINT ( 'NONE',  ( -13.30102111233071760, 76.84881920128778177, -2.309297776588126627 ) ) ;
#3971 = CARTESIAN_POINT ( 'NONE',  ( -9.859355752153115660, 80.28820049829310790, 9.232342221173379215 ) ) ;
#3972 = CARTESIAN_POINT ( 'NONE',  ( 7.500000000000000000, 103.1860286984271795, -9.367496997597600128 ) ) ;
#3973 = DIRECTION ( 'NONE',  ( 0.000000000000000000, 0.000000000000000000, -1.000000000000000000 ) ) ;
#3974 = CARTESIAN_POINT ( 'NONE',  ( -9.520470885617717371, 7.230000000000014637, 6.917026985038133624 ) ) ;
#3975 = CARTESIAN_POINT ( 'NONE',  ( 11.76794919243112680, 49.57999999999999119, -3.823638476888993942 ) ) ;
#3976 = CARTESIAN_POINT ( 'NONE',  ( -11.37500000000000178, -67.67499999999981242, -9.545674412382054647E-13 ) ) ;
#3977 = CARTESIAN_POINT ( 'NONE',  ( 7.714727599200458030, -36.42187499999990763, -18.62499999999934985 ) ) ;
#3978 = CARTESIAN_POINT ( 'NONE',  ( 8.343458848123578520, -9.020000000000008455, 11.48378591275254124 ) ) ;
#3979 = CARTESIAN_POINT ( 'NONE',  ( -2.854184389239543762, 34.28262590607400995, -13.19500222631561037 ) ) ;
#3980 = CARTESIAN_POINT ( 'NONE',  ( 12.05584393367779406, 75.65379272059647064, -6.075093657815592074 ) ) ;
#3981 = CARTESIAN_POINT ( 'NONE',  ( 1.653273178848926472E-15, 80.93000000000000682, 13.50000000000000000 ) ) ;
#3982 = CARTESIAN_POINT ( 'NONE',  ( -7.576616670048093940E-16, 36.67999999999999972, 12.37355403259654985 ) ) ;
#3983 = CARTESIAN_POINT ( 'NONE',  ( -4.765598480478985266, 41.50834662332702862, 12.63248701834810639 ) ) ;
#3984 = CARTESIAN_POINT ( 'NONE',  ( -5.773622420134949529, 58.39004374645310946, -12.20308674553266925 ) ) ;
#3985 = CARTESIAN_POINT ( 'NONE',  ( 2.941637194391252041, 44.78576598995574898, 13.17562406899208405 ) ) ;
#3986 = EDGE_CURVE ( 'NONE', #13703, #13982, #15361, .T. ) ;
#3987 = DIRECTION ( 'NONE',  ( 0.000000000000000000, -1.000000000000000000, 0.000000000000000000 ) ) ;
#3988 = DIRECTION ( 'NONE',  ( 0.000000000000000000, 0.000000000000000000, 1.000000000000000000 ) ) ;
#3989 = CARTESIAN_POINT ( 'NONE',  ( -7.389574489282211722, 55.45617881592348652, -11.29799270601480288 ) ) ;
#3990 = CARTESIAN_POINT ( 'NONE',  ( -13.26124712707118825, 49.84090803523835689, -2.527720896449040744 ) ) ;
#3991 = CARTESIAN_POINT ( 'NONE',  ( 12.75440868670226813, 63.58958983645529628, -4.424554037362297798 ) ) ;
#3992 = CARTESIAN_POINT ( 'NONE',  ( 11.18391117983416372, 42.71430389940879735, -7.561094431090153556 ) ) ;
#3993 = CARTESIAN_POINT ( 'NONE',  ( 13.48029845638929558, 39.45517033420289010, -0.7296389357882047122 ) ) ;
#3994 = ORIENTED_EDGE ( 'NONE', *, *, #13862, .F. ) ;
#3995 = CARTESIAN_POINT ( 'NONE',  ( -12.63529163522881227, 70.75760609934009437, -4.760530200637639098 ) ) ;
#3996 = CARTESIAN_POINT ( 'NONE',  ( -8.343458848123578520, 48.48000000000000398, -11.48378591275254124 ) ) ;
#3997 = VERTEX_POINT ( 'NONE', #15093 ) ;
#3998 = ORIENTED_EDGE ( 'NONE', *, *, #14625, .T. ) ;
#3999 = CARTESIAN_POINT ( 'NONE',  ( -8.343458848123582072, 20.38000000000000256, 11.48378591275254124 ) ) ;
#4000 = CARTESIAN_POINT ( 'NONE',  ( -18.62500000000000000, -41.62499999999990052, -1.562973063126292555E-12 ) ) ;
#4001 = CARTESIAN_POINT ( 'NONE',  ( 6.523056816745746112, 47.91989408141689921, 11.81980764766238501 ) ) ;
#4002 = CARTESIAN_POINT ( 'NONE',  ( 10.92172942406178926, 10.13000000000000078, 7.935100905948385908 ) ) ;
#4003 = CARTESIAN_POINT ( 'NONE',  ( 10.67056894037764359, 72.11562701491169491, 8.269762857265360978 ) ) ;
#4004 = CARTESIAN_POINT ( 'NONE',  ( 12.37411402100152458, 57.62708032287364546, -5.397352088785305924 ) ) ;
#4005 = CARTESIAN_POINT ( 'NONE',  ( 11.76794919243112680, 64.57999999999999829, -3.823638476888993942 ) ) ;
#4006 = CARTESIAN_POINT ( 'NONE',  ( 4.171729424061789260, 34.82999999999999829, 12.83926296998457417 ) ) ;
#4007 = CARTESIAN_POINT ( 'NONE',  ( -11.76794919243112325, 80.93000000000000682, -2.882316262207890869E-15 ) ) ;
#4008 = VECTOR ( 'NONE', #9943, 1000.000000000000000 ) ;
#4009 = CARTESIAN_POINT ( 'NONE',  ( -3.320277394660133385, 47.56063789249560614, 13.08648027329329544 ) ) ;
#4010 = PRODUCT_DEFINITION_CONTEXT ( 'detailed design', #16226, 'design' ) ;
#4011 = CARTESIAN_POINT ( 'NONE',  ( -5.441113646577662166, 5.918584287042170544, 25.42428528562851042 ) ) ;
#4012 = CARTESIAN_POINT ( 'NONE',  ( -1.403940416332137451E-13, 0.000000000000000000, 19.99999999999999289 ) ) ;
#4013 = DIRECTION ( 'NONE',  ( 1.000000000000000000, -1.156482317317871133E-15, 0.000000000000000000 ) ) ;
#4014 = CARTESIAN_POINT ( 'NONE',  ( 8.043339635996300530, -31.21874999999992539, 8.043339635997654113 ) ) ;
#4015 = CARTESIAN_POINT ( 'NONE',  ( 17.42428528562844292, 5.918584287042172321, 19.29752010712858024 ) ) ;
#4016 = CARTESIAN_POINT ( 'NONE',  ( 13.48828357174217807, 33.44935985554970870, -0.5623287429662219283 ) ) ;
#4017 = CARTESIAN_POINT ( 'NONE',  ( -7.790051440343440881, 73.47356962630189514, -11.02593981657268607 ) ) ;
#4018 = VERTEX_POINT ( 'NONE', #16786 ) ;
#4019 = VERTEX_POINT ( 'NONE', #11237 ) ;
#4020 = CARTESIAN_POINT ( 'NONE',  ( -11.76794919243112325, 78.07999999999999829, 3.823638476888994830 ) ) ;
#4021 = ORIENTED_EDGE ( 'NONE', *, *, #15801, .F. ) ;
#4022 = CIRCLE ( 'NONE', #11087, 4.000000000000004441 ) ;
#4023 = CARTESIAN_POINT ( 'NONE',  ( 4.711679271993006957, -70.72812499999983515, 11.37500000000039257 ) ) ;
#4024 = CARTESIAN_POINT ( 'NONE',  ( -6.570750217010064453, 44.43812314528702245, 11.79549799968171264 ) ) ;
#4025 = CARTESIAN_POINT ( 'NONE',  ( 8.178053476330042315, 7.956441929884681130, 16.47733079524786248 ) ) ;
#4026 = CARTESIAN_POINT ( 'NONE',  ( -10.92172942406178926, 40.63000000000000256, -7.935100905948389460 ) ) ;
#4027 = CARTESIAN_POINT ( 'NONE',  ( -13.49970439451574400, 70.94072343917298440, 0.3103739863738418370 ) ) ;
#4028 = CIRCLE ( 'NONE', #13066, 6.000000000000001776 ) ;
#4029 = CARTESIAN_POINT ( 'NONE',  ( -18.62499999999935341, -16.68437499999993889, -7.714727599200458030 ) ) ;
#4030 = CARTESIAN_POINT ( 'NONE',  ( -13.35263207532700669, 67.86002430682577824, -1.997692355781490292 ) ) ;
#4031 = CARTESIAN_POINT ( 'NONE',  ( -18.62499999999935341, -0.03437499999998146899, -7.714727599200458030 ) ) ;
#4032 = CARTESIAN_POINT ( 'NONE',  ( 11.55530260182779401, 54.69032320486194010, -6.980335635328147603 ) ) ;
#4033 = CARTESIAN_POINT ( 'NONE',  ( -9.520470885617717371, 16.22999999999999332, 6.917026985038133624 ) ) ;
#4034 = CARTESIAN_POINT ( 'NONE',  ( -13.16986379960055231, -93.65624999999977263, 13.16986379959834252 ) ) ;
#4035 = CARTESIAN_POINT ( 'NONE',  ( -12.17476046333273842, 64.71527778992695801, -5.849856061721414591 ) ) ;
#4036 = CARTESIAN_POINT ( 'NONE',  ( -13.34634384165835286, 35.00116161489640376, 2.031037000000563530 ) ) ;
#4037 = EDGE_LOOP ( 'NONE', ( #1893, #5555 ) ) ;
#4038 = CARTESIAN_POINT ( 'NONE',  ( -8.048508853266335805, 2.177477983142712198E-15, -9.806701840662514158 ) ) ;
#4039 = CARTESIAN_POINT ( 'NONE',  ( -1.091948754393482712, 31.21923308297253286, -13.45827295822001091 ) ) ;
#4040 = CARTESIAN_POINT ( 'NONE',  ( 3.141418519012163291, 73.06704652263337607, -13.13050367329915602 ) ) ;
#4041 = CARTESIAN_POINT ( 'NONE',  ( -11.76794919243112325, -11.22000000000000242, -3.823638476888998827 ) ) ;
#4042 = FACE_OUTER_BOUND ( 'NONE', #5955, .T. ) ;
#4043 = EDGE_CURVE ( 'NONE', #12592, #13217, #1861, .T. ) ;
#4044 = CARTESIAN_POINT ( 'NONE',  ( 4.171729424061791924, -3.970000000000001528, -12.83926296998457239 ) ) ;
#4045 = CARTESIAN_POINT ( 'NONE',  ( -11.99931260044677472, 53.15821574507319269, 6.186054099126281791 ) ) ;
#4046 = CARTESIAN_POINT ( 'NONE',  ( -11.76794919243112325, 44.92999999999999972, -2.882316262207890869E-15 ) ) ;
#4047 = PRODUCT_CONTEXT ( 'NONE', #13204, 'mechanical' ) ;
#4048 = CARTESIAN_POINT ( 'NONE',  ( 13.49999999999999822, 65.28000000000000114, 4.386415899144237684 ) ) ;
#4049 = CARTESIAN_POINT ( 'NONE',  ( 4.993261676203598398, 50.86016716623841916, 12.54262158262842597 ) ) ;
#4050 = CARTESIAN_POINT ( 'NONE',  ( -11.34510250317683600, 37.65566839993009296, -7.320287091699782422 ) ) ;
#4051 = CARTESIAN_POINT ( 'NONE',  ( 4.208051776087926577, 35.83130703551096019, 12.82741174251338023 ) ) ;
#4052 = CARTESIAN_POINT ( 'NONE',  ( -1.564113515457998370E-12, -19.73749999999997229, 18.62500000000000000 ) ) ;
#4053 = CARTESIAN_POINT ( 'NONE',  ( -12.95509469782950873, 74.06591892939171373, 3.797696039018899405 ) ) ;
#4054 = CARTESIAN_POINT ( 'NONE',  ( -12.95329468731883260, 76.79322173300190002, -3.819660872089479575 ) ) ;
#4055 = CARTESIAN_POINT ( 'NONE',  ( -11.14889335015297966, 80.21642165902807164, 7.613376886237952057 ) ) ;
#4056 = CARTESIAN_POINT ( 'NONE',  ( -2.648919002463483441, 80.93000000000000682, 12.65678160791643592 ) ) ;
#4057 = CARTESIAN_POINT ( 'NONE',  ( -8.343458848123582072, 8.380000000000002558, 11.48378591275253768 ) ) ;
#4058 = CARTESIAN_POINT ( 'NONE',  ( 9.520470885617717371, 2.730000000000010196, -6.917026985038131848 ) ) ;
#4059 = CARTESIAN_POINT ( 'NONE',  ( -7.272992578804307939, 47.47999999999999687, -10.01041549318727064 ) ) ;
#4060 = CARTESIAN_POINT ( 'NONE',  ( 11.37500000000000000, -49.94999999999988205, 9.531744055041752924E-13 ) ) ;
#4061 = CARTESIAN_POINT ( 'NONE',  ( -18.62500000000064659, -26.01562499999994671, 7.714727599197335195 ) ) ;
#4062 =( BOUNDED_CURVE ( )  B_SPLINE_CURVE ( 2, ( #4146, #262, #7163, #12632, #2891, #16599, #8323, #1575, #6993, #4506, #15260, #12368, #16237 ),
 .UNSPECIFIED., .F., .F. ) 
 B_SPLINE_CURVE_WITH_KNOTS ( ( 3, 2, 2, 2, 2, 2, 3 ),
 ( 0.5972222222222222099, 0.5999999999999999778, 0.6055555555555555136, 0.6111111111111111605, 0.6166666666666666963, 0.6222222222222222321, 0.6250000000000000000 ),
 .UNSPECIFIED. ) 
 CURVE ( )  GEOMETRIC_REPRESENTATION_ITEM ( )  RATIONAL_B_SPLINE_CURVE ( ( 0.9755282581475768211, 0.9755282581475768211, 1.000000000000000000, 0.9510565162951535312, 1.000000000000000000, 0.9510565162951535312, 1.000000000000000000, 0.9510565162951535312, 1.000000000000000000, 0.9510565162951535312, 1.000000000000000000, 0.9755282581475768211, 0.9755282581475768211 ) ) 
 REPRESENTATION_ITEM ( '' )  );
#4063 = CARTESIAN_POINT ( 'NONE',  ( -10.92172942406178926, -7.369999999999994778, -7.935100905948389460 ) ) ;
#4064 = CARTESIAN_POINT ( 'NONE',  ( -9.612436902512136783, 40.55921212120037467, -9.485869169573415860 ) ) ;
#4065 = FACE_OUTER_BOUND ( 'NONE', #17444, .T. ) ;
#4066 = CARTESIAN_POINT ( 'NONE',  ( 10.31463346427486982, 75.09593381292602032, 8.709679962864647962 ) ) ;
#4067 = EDGE_CURVE ( 'NONE', #7126, #16308, #16542, .T. ) ;
#4068 = FACE_OUTER_BOUND ( 'NONE', #6557, .T. ) ;
#4069 = CARTESIAN_POINT ( 'NONE',  ( 11.76794919243112680, 40.57999999999999829, -3.823638476888993942 ) ) ;
#4070 = CARTESIAN_POINT ( 'NONE',  ( -11.18770039063602262, 41.21406332147840601, 7.555487409198383908 ) ) ;
#4071 = CARTESIAN_POINT ( 'NONE',  ( -11.07316193868316390, 58.63892660121854306, -7.722844086540342268 ) ) ;
#4072 = CARTESIAN_POINT ( 'NONE',  ( -3.708203932499367195, 9.196025403784441110, -11.41267819554184548 ) ) ;
#4073 = DIRECTION ( 'NONE',  ( 0.000000000000000000, 1.000000000000000000, 0.000000000000000000 ) ) ;
#4074 = CARTESIAN_POINT ( 'NONE',  ( -7.416407864998739718, 4.513974596215559743, 10.20780970022447853 ) ) ;
#4075 = DIRECTION ( 'NONE',  ( -1.772429021826857464E-16, 1.000000000000000000, 0.000000000000000000 ) ) ;
#4076 = CARTESIAN_POINT ( 'NONE',  ( -6.405441672365779660, 49.41516637713032623, -11.88598892033222398 ) ) ;
#4077 = CARTESIAN_POINT ( 'NONE',  ( 13.50050750903061747, 63.42343654352898596, 0.1847079823050248870 ) ) ;
#4078 = CARTESIAN_POINT ( 'NONE',  ( 10.28321627186559262, 42.76572808278937998, -8.746763802038561408 ) ) ;
#4079 = CARTESIAN_POINT ( 'NONE',  ( 4.245544141064997667, 38.83265899993158854, 12.81504996667835883 ) ) ;
#4080 = ORIENTED_EDGE ( 'NONE', *, *, #17466, .T. ) ;
#4081 = CARTESIAN_POINT ( 'NONE',  ( 2.445080149700053643E-15, 75.17999999999999261, -13.50000000000000000 ) ) ;
#4082 = CARTESIAN_POINT ( 'NONE',  ( 4.711679271993006068, -13.52812499999996909, 11.37500000000039257 ) ) ;
#4083 = CARTESIAN_POINT ( 'NONE',  ( 10.92172942406178926, 12.13000000000000256, 7.935100905948385908 ) ) ;
#4084 = ORIENTED_EDGE ( 'NONE', *, *, #14767, .T. ) ;
#4085 = CARTESIAN_POINT ( 'NONE',  ( -5.834127350457870342, 43.39242430467762546, -12.17494074988466224 ) ) ;
#4086 = CARTESIAN_POINT ( 'NONE',  ( -18.62500000000064659, -42.66562499999989200, 7.714727599197335195 ) ) ;
#4087 = CARTESIAN_POINT ( 'NONE',  ( 9.331600089522767760, 60.81473193213921036, -9.755580554834571316 ) ) ;
#4088 = PRODUCT ( 'Base', 'Base', '', ( #6714 ) ) ;
#4089 = CARTESIAN_POINT ( 'NONE',  ( -10.92172942406178926, 14.63000000000000433, -7.935100905948389460 ) ) ;
#4090 = ADVANCED_FACE ( 'NONE', ( #11063 ), #4339, .F. ) ;
#4091 = CARTESIAN_POINT ( 'NONE',  ( -1.010931998681471075E-07, 71.67999718330101189, 13.49999999999999822 ) ) ;
#4092 = CARTESIAN_POINT ( 'NONE',  ( 11.62061665277031075, 57.68594776230959553, -6.871996344357341080 ) ) ;
#4093 = CARTESIAN_POINT ( 'NONE',  ( -3.636496289402155746, 72.53000000000000114, 11.19198476289190936 ) ) ;
#4094 = CARTESIAN_POINT ( 'NONE',  ( -7.272992578804307939, 77.48000000000000398, -10.01041549318726886 ) ) ;
#4095 = CARTESIAN_POINT ( 'NONE',  ( -7.033908694595895739, 47.41891739858513688, 11.52279350434594285 ) ) ;
#4096 = DIRECTION ( 'NONE',  ( 0.000000000000000000, 0.000000000000000000, -1.000000000000000000 ) ) ;
#4097 = CARTESIAN_POINT ( 'NONE',  ( 0.3512640400060710877, 8.055266896996085890, -18.02316420754752713 ) ) ;
#4098 = CARTESIAN_POINT ( 'NONE',  ( 2.107853069822502790E-14, 31.18000000000000682, -13.50000000000000000 ) ) ;
#4099 = CARTESIAN_POINT ( 'NONE',  ( -5.620581134510726606, 56.47591212409395922, 12.27434859643074994 ) ) ;
#4100 = CARTESIAN_POINT ( 'NONE',  ( 4.711679271994909435, -3.121874999999992184, -11.37499999999960387 ) ) ;
#4101 = CARTESIAN_POINT ( 'NONE',  ( 10.92172942406178926, 6.129999999999996341, 7.935100905948385908 ) ) ;
#4102 = CARTESIAN_POINT ( 'NONE',  ( 10.71824045277809923, 33.74192371909632016, -8.219471766505868970 ) ) ;
#4103 = CARTESIAN_POINT ( 'NONE',  ( -3.211247102494231953, 73.29552755700889577, -13.11374676138101947 ) ) ;
#4104 = DIRECTION ( 'NONE',  ( -0.000000000000000000, -1.000000000000000000, -0.000000000000000000 ) ) ;
#4105 = ORIENTED_EDGE ( 'NONE', *, *, #9055, .F. ) ;
#4106 = CARTESIAN_POINT ( 'NONE',  ( 11.76794919243112325, 23.28000000000000114, 3.823638476888996163 ) ) ;
#4107 = CARTESIAN_POINT ( 'NONE',  ( -4.830293611773615048, 62.50587364081614083, 12.60858922533637205 ) ) ;
#4108 = AXIS2_PLACEMENT_3D ( 'NONE', #14580, #3813, #2550 ) ;
#4109 = ORIENTED_EDGE ( 'NONE', *, *, #4375, .T. ) ;
#4110 = CARTESIAN_POINT ( 'NONE',  ( -13.47828624137987497, 40.90358342329059127, -0.7654979494148171915 ) ) ;
#4111 = CARTESIAN_POINT ( 'NONE',  ( 11.37499999999999645, -73.84999999999983800, 9.531744055041752924E-13 ) ) ;
#4112 = CARTESIAN_POINT ( 'NONE',  ( -11.20659543516484469, 44.21289395307379522, 7.527431242496333219 ) ) ;
#4113 = CARTESIAN_POINT ( 'NONE',  ( -7.499999999999996447, -27.18121722713999944, 5.064597142177448497 ) ) ;
#4114 = CARTESIAN_POINT ( 'NONE',  ( 10.92172942406178926, 45.12999999999999545, 7.935100905948387684 ) ) ;
#4115 = CARTESIAN_POINT ( 'NONE',  ( 8.343458848123583849, 44.87999999999998835, -11.48378591275253768 ) ) ;
#4116 = CARTESIAN_POINT ( 'NONE',  ( -12.93889380315461501, 71.06794844313003523, 3.851678986249745140 ) ) ;
#4117 = AXIS2_PLACEMENT_3D ( 'NONE', #7077, #12280, #16422 ) ;
#4118 = CARTESIAN_POINT ( 'NONE',  ( 1.561832610794586740E-12, -13.56249999999995026, -18.62500000000000000 ) ) ;
#4119 = CARTESIAN_POINT ( 'NONE',  ( -13.43488328562637513, 67.88398595381684686, -1.324420451639741092 ) ) ;
#4120 = CARTESIAN_POINT ( 'NONE',  ( 13.16986379960055054, -85.33124999999978400, -13.16986379959834430 ) ) ;
#4121 = CARTESIAN_POINT ( 'NONE',  ( 11.39185320920821809, 54.70104879577822743, -7.245458119857994816 ) ) ;
#4122 = CARTESIAN_POINT ( 'NONE',  ( 0.000000000000000000, 9.000000000000000000, 0.000000000000000000 ) ) ;
#4123 = EDGE_CURVE ( 'NONE', #4640, #8734, #10328, .T. ) ;
#4124 = CARTESIAN_POINT ( 'NONE',  ( -13.46072377650594376, 64.89438511582379476, -1.029100581260686376 ) ) ;
#4125 = ORIENTED_EDGE ( 'NONE', *, *, #1840, .T. ) ;
#4126 = CARTESIAN_POINT ( 'NONE',  ( -13.49476282772579694, 34.91482293905653478, -0.4351865453969105402 ) ) ;
#4127 = CARTESIAN_POINT ( 'NONE',  ( 2.621994543952811015E-15, 20.17999999999999261, -14.19474002721660355 ) ) ;
#4128 = ORIENTED_EDGE ( 'NONE', *, *, #4596, .F. ) ;
#4129 = DIRECTION ( 'NONE',  ( 0.000000000000000000, 0.000000000000000000, -1.000000000000000000 ) ) ;
#4130 = CARTESIAN_POINT ( 'NONE',  ( 7.500000000000000888, -22.00000000000000000, 9.367496997597600128 ) ) ;
#4131 = CARTESIAN_POINT ( 'NONE',  ( 7.696945099050856776, 72.89056765019519446, -11.09520446863491827 ) ) ;
#4132 = CARTESIAN_POINT ( 'NONE',  ( 7.272992578804311492, -9.120000000000004547, -10.01041549318726709 ) ) ;
#4133 = CARTESIAN_POINT ( 'NONE',  ( 0.07359788859287424989, 79.17735392238709835, -13.49981184443148408 ) ) ;
#4134 = CARTESIAN_POINT ( 'NONE',  ( 13.49999999999999822, -13.72000000000000419, 4.386415899144237684 ) ) ;
#4135 = CARTESIAN_POINT ( 'NONE',  ( -8.343458848123576743, 76.48000000000001819, -11.48378591275254301 ) ) ;
#4136 = CARTESIAN_POINT ( 'NONE',  ( -12.16582101725930265, 52.71440321287756348, -5.873394938063603021 ) ) ;
#4137 = CARTESIAN_POINT ( 'NONE',  ( -11.76794919243112325, 47.92999999999999972, -2.882316262207890869E-15 ) ) ;
#4138 = CARTESIAN_POINT ( 'NONE',  ( 12.50102360570146942, 51.24461652421468472, 5.096535108048335871 ) ) ;
#4139 = CARTESIAN_POINT ( 'NONE',  ( -5.545884925436540769, 37.38119561285134296, -12.30826441516979664 ) ) ;
#4140 = CARTESIAN_POINT ( 'NONE',  ( 4.003383602335978786, 35.82394118477286327, 12.89283635254156835 ) ) ;
#4141 = CARTESIAN_POINT ( 'NONE',  ( 18.62500000000064659, -8.290625000000000355, -7.714727599197336083 ) ) ;
#4142 = CARTESIAN_POINT ( 'NONE',  ( -12.11092945869762438, 74.14939596029618940, 5.964972250005902588 ) ) ;
#4143 = CARTESIAN_POINT ( 'NONE',  ( -11.21515498128762900, 76.64763740971592654, -7.514674283766924923 ) ) ;
#4144 = CARTESIAN_POINT ( 'NONE',  ( -10.57611007270270065, 80.24971877258465724, 8.393134611178751925 ) ) ;
#4145 = CARTESIAN_POINT ( 'NONE',  ( -7.272992578804310604, 13.37999999999999012, 10.01041549318726709 ) ) ;
#4146 = CARTESIAN_POINT ( 'NONE',  ( -8.891200544363830713E-16, 1.546025403784439423, 12.00000000000000000 ) ) ;
#4147 = DIRECTION ( 'NONE',  ( 1.000000000000000000, 0.000000000000000000, -1.224646799147353207E-16 ) ) ;
#4148 = DIRECTION ( 'NONE',  ( 0.000000000000000000, 0.000000000000000000, -1.000000000000000000 ) ) ;
#4149 = CARTESIAN_POINT ( 'NONE',  ( -11.76794919243112325, 0.7799999999999955858, -3.823638476888998827 ) ) ;
#4150 = CARTESIAN_POINT ( 'NONE',  ( 11.76794919243112325, 46.27999999999999403, 3.823638476888997051 ) ) ;
#4151 = CARTESIAN_POINT ( 'NONE',  ( 7.714727599197338748, -13.52812499999996732, 18.62500000000063949 ) ) ;
#4152 = CARTESIAN_POINT ( 'NONE',  ( 4.171729424061791924, -10.96999999999999353, -12.83926296998457239 ) ) ;
#4153 = CARTESIAN_POINT ( 'NONE',  ( -10.37886156279672889, 40.59931919632202124, -8.633337318100664959 ) ) ;
#4154 = CARTESIAN_POINT ( 'NONE',  ( 6.750022862106050958, 30.59592842876635643, 11.69132975161703492 ) ) ;
#4155 = CARTESIAN_POINT ( 'NONE',  ( 11.44075521902680670, 75.16203548088178366, 7.166853402732320077 ) ) ;
#4156 = CARTESIAN_POINT ( 'NONE',  ( 4.905322627110114908, 5.715075095792292317E-16, -15.60939936909243819 ) ) ;
#4157 = CARTESIAN_POINT ( 'NONE',  ( 3.636496289402157078, 35.03000000000000114, -11.19198476289190936 ) ) ;
#4158 = CARTESIAN_POINT ( 'NONE',  ( -3.648845442435871611, 41.54898592542676283, 13.00161767624870457 ) ) ;
#4159 = CARTESIAN_POINT ( 'NONE',  ( -5.854979236895436756, 58.39324858652572914, -12.16430431366758569 ) ) ;
#4160 = CARTESIAN_POINT ( 'NONE',  ( 0.000000000000000000, 9.000000000000000000, 0.000000000000000000 ) ) ;
#4161 = APPLICATION_CONTEXT ( 'automotive_design' ) ;
#4162 = CARTESIAN_POINT ( 'NONE',  ( -22.26879735319533893, 6.548268786306344680, 7.999999999999786837 ) ) ;
#4163 = DIRECTION ( 'NONE',  ( -0.8660254037844393737, -0.000000000000000000, 0.4999999999999986122 ) ) ;
#4164 = CARTESIAN_POINT ( 'NONE',  ( -0.1475770875894988898, 55.18530632762605848, -13.50000000041324100 ) ) ;
#4165 = EDGE_CURVE ( 'NONE', #16001, #14960, #14783, .T. ) ;
#4166 = CARTESIAN_POINT ( 'NONE',  ( -10.18460302888335534, 49.58894042909286526, -8.861442684701360761 ) ) ;
#4167 = CARTESIAN_POINT ( 'NONE',  ( 13.25541523722283266, 63.33835930678574755, 2.600118167593814977 ) ) ;
#4168 = CARTESIAN_POINT ( 'NONE',  ( 13.45911878322305277, 42.46696013891686050, -1.067321996712556897 ) ) ;
#4169 = CARTESIAN_POINT ( 'NONE',  ( 7.123418755682585868, 38.94487885092864587, 11.46980419701936249 ) ) ;
#4170 = EDGE_LOOP ( 'NONE', ( #2151, #1354, #2779, #11010 ) ) ;
#4171 = CARTESIAN_POINT ( 'NONE',  ( -12.00000000000000178, 3.946025403784445551, 3.899036354794875869 ) ) ;
#4172 = CARTESIAN_POINT ( 'NONE',  ( -2.138189944381236884, 48.25688142232026223, -13.50000000000000000 ) ) ;
#4173 = CARTESIAN_POINT ( 'NONE',  ( -10.92172942406179104, 11.23000000000000398, 7.935100905948385908 ) ) ;
#4174 = ORIENTED_EDGE ( 'NONE', *, *, #16694, .F. ) ;
#4175 = B_SPLINE_CURVE_WITH_KNOTS ( 'NONE', 3,
 ( #4689, #13944, #703, #8680, #10092, #8768, #11494, #13158, #6455, #2610, #1044, #2354, #13408, #15880, #11840, #17389, #14465, #7786, #5036, #11922, #9113, #2526, #5127, #13325, #10770, #1132, #7955, #2265, #9201, #17127, #17216, #6543, #14722, #13071, #956, #14639, #1217, #11751, #2436, #3871, #7868, #10517, #8041, #3960, #5215, #1297, #14552, #9021, #3609, #3788, #6628, #13243, #10434, #5385, #6712, #15793, #17302, #17472, #10603, #5304, #15968, #9287, #12007, #14377, #10686, #16052, #9372, #7692, #6368, #12089, #3700, #4045, #164, #4223, #16317, #16499, #1650, #14807, #7066, #16410, #9637, #12535, #5829, #12448, #5568, #9459, #10950, #14986, #2878, #4403, #333, #2701, #5742, #421, #9813, #14897, #7150, #11124, #2968, #15159, #8222, #8129, #13495, #3058, #5476, #8486, #1562, #1384, #8397, #2791, #6801, #10857, #1737, #16133, #13583, #15068, #12179, #13751, #13837, #70, #12357, #16225, #4136, #9548, #1476, #6893, #5656, #12266, #8311, #13666, #6982, #4311, #251, #11038, #9723, #12882, #3332, #10074, #9901, #6005, #16851, #16760, #10242, #7233, #4580, #11475, #3238, #14014, #15596, #8659, #9987, #3503, #11387, #1906, #7501, #15335, #7323, #12620, #1989, #16674, #16936, #12707, #3421, #847, #8747, #15509, #15248, #4667, #508, #594, #14104, #4839, #3146, #8571, #4753, #8835, #1818, #15425, #10159, #7414, #5916, #8918, #11561, #12796, #14276 ),
 .UNSPECIFIED., .F., .F.,
 ( 4, 2, 2, 1, 1, 2, 2, 2, 2, 1, 2, 2, 1, 1, 2, 2, 2, 1, 1, 2, 2, 1, 2, 2, 2, 2, 2, 1, 2, 2, 1, 2, 2, 2, 1, 1, 2, 2, 1, 2, 2, 2, 2, 1, 1, 2, 2, 1, 2, 2, 1, 2, 2, 1, 2, 2, 1, 1, 1, 1, 2, 2, 2, 1, 1, 1, 1, 2, 2, 2, 2, 2, 1, 2, 2, 2, 2, 2, 1, 1, 1, 2, 2, 1, 2, 2, 1, 1, 2, 2, 1, 2, 2, 2, 2, 1, 1, 2, 2, 1, 1, 1, 2, 2, 2, 2, 1, 2, 2, 1, 2, 2, 4 ),
 ( 0.5344080644574688010, 0.5345226381220460343, 0.5345512815381903149, 0.5345799249543345955, 0.5346372117866232676, 0.5348663591157777342, 0.5353246537740865563, 0.5362412430907044225, 0.5366995377490133556, 0.5369286850781678222, 0.5370432587427450555, 0.5370719021588893360, 0.5371005455750336166, 0.5371578324073221777, 0.5380744217239400440, 0.5389910110405577992, 0.5394493056988667323, 0.5395065925311554045, 0.5395352359472996850, 0.5395495576553718253, 0.5395567185094078955, 0.5395638793634439656, 0.5396784530280211989, 0.5399076003571755544, 0.5408241896737931986, 0.5417407789904108428, 0.5419699263195651984, 0.5420272131518538705, 0.5420415348599260108, 0.5420558565679981511, 0.5420844999841424317, 0.5421990736487196649, 0.5426573683070287091, 0.5431156629653376422, 0.5432302366299148755, 0.5432875234622035476, 0.5433018451702756879, 0.5433161668783478282, 0.5433448102944922198, 0.5435739576236466863, 0.5444905469402646636, 0.5445478337725533358, 0.5446051206048420079, 0.5447196942694192412, 0.5449488415985737078, 0.5454071362568827519, 0.5463237255735007292, 0.5467820202318096623, 0.5470111675609642399, 0.5470684543932528010, 0.5471257412255414732, 0.5472403148901187064, 0.5481569042067366837, 0.5482714778713139170, 0.5483001212874583086, 0.5483144429955304489, 0.5483287647036025891, 0.5483860515358911503, 0.5486151988650457278, 0.5490734935233547720, 0.5495317881816637051, 0.5495604315978080967, 0.5495675924518441668, 0.5495747533058802370, 0.5495890750139523773, 0.5496463618462410494, 0.5497609355108182827, 0.5499900828399727493, 0.5509066721565909486, 0.5518232614732090369, 0.5520524088023635034, 0.5521096956346521756, 0.5521669824669407367, 0.5522815561315180810, 0.5527398507898271252, 0.5536564401064452134, 0.5541147347647542576, 0.5543438820939088352, 0.5544584557584860685, 0.5545157425907747406, 0.5545443860069190212, 0.5545587077149911615, 0.5545658685690272316, 0.5545730294230633017, 0.5564062080562987012, 0.5568645027146076343, 0.5569790763791848676, 0.5570363632114734287, 0.5570650066276177093, 0.5570793283356898495, 0.5570936500437619898, 0.5573227973729164564, 0.5582393866895342116, 0.5591559760061519668, 0.5593851233353063224, 0.5594996969998835556, 0.5595569838321722278, 0.5595641446862082979, 0.5595713055402443681, 0.5595856272483165084, 0.5596142706644607889, 0.5600725653227697221, 0.5605308599810786552, 0.5607600073102330107, 0.5609891546393874773, 0.5619057439560052325, 0.5620203176205824658, 0.5620489610367268574, 0.5620776044528711379, 0.5621348912851596991, 0.5623640386143141656, 0.5628223332726230987, 0.5637389225892408540 ),
 .UNSPECIFIED. ) ;
#4176 = CARTESIAN_POINT ( 'NONE',  ( -4.364754663317498284, 43.33701438703417352, -12.77552687514723928 ) ) ;
#4177 = CARTESIAN_POINT ( 'NONE',  ( -7.500000000000000000, 108.7270211387039183, -1.010069558262743028 ) ) ;
#4178 = CARTESIAN_POINT ( 'NONE',  ( 12.99687134794458920, 60.56044921522202884, -3.651220384438404576 ) ) ;
#4179 = CARTESIAN_POINT ( 'NONE',  ( -8.343458848123576743, 11.48000000000000398, -11.48378591275254301 ) ) ;
#4180 = CARTESIAN_POINT ( 'NONE',  ( 7.714727599200458030, -19.77187499999995168, -18.62499999999935341 ) ) ;
#4181 = CARTESIAN_POINT ( 'NONE',  ( 13.40455306696748927, 66.48586035906389213, -1.602499198163928273 ) ) ;
#4182 = CARTESIAN_POINT ( 'NONE',  ( 3.256375548821571542, 56.79708330500473323, 13.10137511577798719 ) ) ;
#4183 = CARTESIAN_POINT ( 'NONE',  ( -11.76794919243112325, 59.92999999999999972, -2.882316262207890869E-15 ) ) ;
#4184 = CARTESIAN_POINT ( 'NONE',  ( 7.272992578804311492, 64.87999999999999545, -10.01041549318726709 ) ) ;
#4185 = CARTESIAN_POINT ( 'NONE',  ( -9.912099458519779915, 47.28536638360703392, 9.165169439464738943 ) ) ;
#4186 = CARTESIAN_POINT ( 'NONE',  ( 5.537792478938636798, 45.97909885940507024, -12.31190230144335906 ) ) ;
#4187 = CARTESIAN_POINT ( 'NONE',  ( 0.000000000000000000, 80.93000000000000682, 0.000000000000000000 ) ) ;
#4188 = CARTESIAN_POINT ( 'NONE',  ( 3.604077478036761484, -100.0000000000000142, 14.28339603699808258 ) ) ;
#4189 = CIRCLE ( 'NONE', #9569, 26.00000000000000355 ) ;
#4190 = CARTESIAN_POINT ( 'NONE',  ( -5.733944026526732074, 10.00000000000000000, -11.46105073991378376 ) ) ;
#4191 = CARTESIAN_POINT ( 'NONE',  ( 8.043339635996300530, -64.51874999999984084, 8.043339635997654113 ) ) ;
#4192 = EDGE_CURVE ( 'NONE', #12894, #14883, #16604, .T. ) ;
#4193 = CYLINDRICAL_SURFACE ( 'NONE', #10084, 4.000000000000003553 ) ;
#4194 = CARTESIAN_POINT ( 'NONE',  ( 13.35406747998390564, 33.36045359896084506, 1.984711021133432896 ) ) ;
#4195 = CARTESIAN_POINT ( 'NONE',  ( 1.775737858763662015E-15, 9.000000000000000000, 14.50000000000000000 ) ) ;
#4196 = CARTESIAN_POINT ( 'NONE',  ( -9.999999999999776179, 7.983052681820796970, -15.32050807568890427 ) ) ;
#4197 = ORIENTED_EDGE ( 'NONE', *, *, #11562, .T. ) ;
#4198 = CARTESIAN_POINT ( 'NONE',  ( -8.343458848123582072, 43.38000000000000256, 11.48378591275253768 ) ) ;
#4199 = VERTEX_POINT ( 'NONE', #7072 ) ;
#4200 = CARTESIAN_POINT ( 'NONE',  ( -13.47061399229918344, 40.89918744336559797, -0.8931361110388874591 ) ) ;
#4201 = CARTESIAN_POINT ( 'NONE',  ( -7.272992578804307939, -14.51999999999999957, -10.01041549318726886 ) ) ;
#4202 = CARTESIAN_POINT ( 'NONE',  ( 18.62499999999935341, -22.85937499999996803, 7.714727599200469577 ) ) ;
#4203 = CARTESIAN_POINT ( 'NONE',  ( -12.08847575587519074, 44.15120909323470499, 6.010142657089093454 ) ) ;
#4204 = CARTESIAN_POINT ( 'NONE',  ( 0.000000000000000000, 3.000000000000000000, 0.000000000000000000 ) ) ;
#4205 = CARTESIAN_POINT ( 'NONE',  ( -8.343458848123582072, 41.38000000000000256, 11.48378591275254124 ) ) ;
#4206 = CARTESIAN_POINT ( 'NONE',  ( -13.42488017928338628, 70.88049257656408031, -1.423317239027405590 ) ) ;
#4207 = CARTESIAN_POINT ( 'NONE',  ( 18.62500000000064659, -43.74062499999988773, -7.714727599197336083 ) ) ;
#4208 = CARTESIAN_POINT ( 'NONE',  ( -1.260278075713701318, 67.22531399419105469, -13.44469158219603422 ) ) ;
#4209 = CARTESIAN_POINT ( 'NONE',  ( 18.62500000000064659, -77.04062499999979252, -7.714727599197336083 ) ) ;
#4210 = CARTESIAN_POINT ( 'NONE',  ( 13.49413416657210085, 54.44402071019561618, -0.4078984894991014576 ) ) ;
#4211 = VECTOR ( 'NONE', #11830, 1000.000000000000114 ) ;
#4212 = CARTESIAN_POINT ( 'NONE',  ( -11.35960375279439738, 64.65661637531263750, -7.297776375780255620 ) ) ;
#4213 = VERTEX_POINT ( 'NONE', #16506 ) ;
#4214 = CARTESIAN_POINT ( 'NONE',  ( -12.66168252233810421, 35.09958735483692749, 4.686808648749069661 ) ) ;
#4215 = ORIENTED_EDGE ( 'NONE', *, *, #617, .T. ) ;
#4216 = CARTESIAN_POINT ( 'NONE',  ( 12.87051123520935825, 78.28367826617611058, 4.074318883512994205 ) ) ;
#4217 = CARTESIAN_POINT ( 'NONE',  ( -1.732050807569007977, 0.000000000000000000, 18.99999999999998224 ) ) ;
#4218 = CARTESIAN_POINT ( 'NONE',  ( -7.845105219487623849, 31.47600457549274466, -10.98698378474273696 ) ) ;
#4219 = CARTESIAN_POINT ( 'NONE',  ( 8.220432041259709166, 72.86719779332030100, -10.70875809315417548 ) ) ;
#4220 = DIRECTION ( 'NONE',  ( -0.8660254037844434816, 0.000000000000000000, 0.4999999999999918399 ) ) ;
#4221 = CARTESIAN_POINT ( 'NONE',  ( 4.171729424061791924, -12.96999999999999531, -12.83926296998457239 ) ) ;
#4222 = CARTESIAN_POINT ( 'NONE',  ( 8.343458848123578520, 71.98000000000000398, 11.48378591275254124 ) ) ;
#4223 = CARTESIAN_POINT ( 'NONE',  ( -12.11224912280836108, 53.14936213474186388, 5.963634143833839829 ) ) ;
#4224 = CIRCLE ( 'NONE', #16348, 4.000000000000000000 ) ;
#4225 = ADVANCED_FACE ( 'NONE', ( #340 ), #5749, .F. ) ;
#4226 = CARTESIAN_POINT ( 'NONE',  ( 11.76794919243112680, 52.57999999999999119, -3.823638476888993942 ) ) ;
#4227 = CARTESIAN_POINT ( 'NONE',  ( -8.691771469529815392E-16, 64.68000000000000682, 14.19474002721660355 ) ) ;
#4228 = DIRECTION ( 'NONE',  ( -0.000000000000000000, -1.000000000000000000, -0.000000000000000000 ) ) ;
#4229 = CARTESIAN_POINT ( 'NONE',  ( 4.953436321318733349, 68.85867169319138270, 12.55852084432367732 ) ) ;
#4230 = CARTESIAN_POINT ( 'NONE',  ( -4.183764169839751190, 37.33043068766654926, -12.83544830047670082 ) ) ;
#4231 = CONICAL_SURFACE ( 'NONE', #16932, 14.50000000000000000, 1.308996938995753867 ) ;
#4232 = CARTESIAN_POINT ( 'NONE',  ( 5.574118405682551014, 35.88201004368047364, 12.30340700596329917 ) ) ;
#4233 = CARTESIAN_POINT ( 'NONE',  ( -7.714727599197334307, -45.75312499999991189, -18.62500000000064659 ) ) ;
#4234 = CARTESIAN_POINT ( 'NONE',  ( -12.73921229380289155, 74.09290750163174266, 4.517609494197782460 ) ) ;
#4235 = PRODUCT_DEFINITION_SHAPE ( 'NONE', 'NONE',  #8388 ) ;
#4236 = CARTESIAN_POINT ( 'NONE',  ( -12.05845239338915320, 76.70338954954424082, -6.158670844540059974 ) ) ;
#4237 = CARTESIAN_POINT ( 'NONE',  ( -4.342137793289712278, 79.33615335351939279, -12.78264298514469210 ) ) ;
#4238 = DIRECTION ( 'NONE',  ( 0.000000000000000000, 1.000000000000000000, 0.000000000000000000 ) ) ;
#4239 = CARTESIAN_POINT ( 'NONE',  ( 10.92172942406179104, 4.730000000000011973, -7.935100905948385908 ) ) ;
#4240 = FILL_AREA_STYLE ('',( #15082 ) ) ;
#4241 = CARTESIAN_POINT ( 'NONE',  ( -9.520470885617715595, 6.629999999999997229, -6.917026985038136289 ) ) ;
#4242 = CARTESIAN_POINT ( 'NONE',  ( 2.272985001014427393E-15, 47.17999999999999972, -12.37355403259654807 ) ) ;
#4243 = CARTESIAN_POINT ( 'NONE',  ( 10.92172942406179104, -17.26999999999999957, -7.935100905948385908 ) ) ;
#4244 = CARTESIAN_POINT ( 'NONE',  ( -1.111710639975107329, 34.21993612021496745, -13.46167583268210244 ) ) ;
#4245 = CARTESIAN_POINT ( 'NONE',  ( 13.48545920529975284, 75.45158341798384072, -0.6264344526569241012 ) ) ;
#4246 = CARTESIAN_POINT ( 'NONE',  ( 3.814188548975826709, -6.916538280674965647E-15, -13.28211646800023082 ) ) ;
#4247 = EDGE_CURVE ( 'NONE', #17099, #2562, #5839, .T. ) ;
#4248 = CARTESIAN_POINT ( 'NONE',  ( -7.272992578804307939, 35.47999999999999687, -10.01041549318726886 ) ) ;
#4249 = CARTESIAN_POINT ( 'NONE',  ( -11.16896011296937985, 41.21521864355013065, 7.583167778474193987 ) ) ;
#4250 = CIRCLE ( 'NONE', #10474, 8.999999999999998224 ) ;
#4251 = CARTESIAN_POINT ( 'NONE',  ( 10.97408553220991578, 51.72700490979467958, -7.865491942308953988 ) ) ;
#4252 = CARTESIAN_POINT ( 'NONE',  ( 5.900366410768304704, 44.89475997489012826, 12.14732960817785390 ) ) ;
#4253 = CARTESIAN_POINT ( 'NONE',  ( 13.50000000000000000, 59.42999999999999972, 1.653273178848926867E-15 ) ) ;
#4254 = CARTESIAN_POINT ( 'NONE',  ( 0.000000000000000000, 3.000000000000000000, 0.000000000000000000 ) ) ;
#4255 = CARTESIAN_POINT ( 'NONE',  ( -2.138189944381279073, 57.25688142232026223, -13.49999999999998579 ) ) ;
#4256 = CARTESIAN_POINT ( 'NONE',  ( -13.07794080639409273, 49.80669500938279270, -3.469076081897399799 ) ) ;
#4257 = CARTESIAN_POINT ( 'NONE',  ( 13.14224245847790584, 63.31794964476952714, 3.160171244385233447 ) ) ;
#4258 = CARTESIAN_POINT ( 'NONE',  ( 13.48432407896599727, 42.40750944205898065, 0.6513807325604739074 ) ) ;
#4259 = CARTESIAN_POINT ( 'NONE',  ( 2.495622557441647960, 38.76969659664788992, 13.26920102393307133 ) ) ;
#4260 = EDGE_LOOP ( 'NONE', ( #6579, #5444 ) ) ;
#4261 = CARTESIAN_POINT ( 'NONE',  ( -2.501400086087330887, 70.26993977764597332, -13.26633446808875405 ) ) ;
#4262 = CARTESIAN_POINT ( 'NONE',  ( -8.891200544363830713E-16, 55.67999999999999972, 13.50000000000000000 ) ) ;
#4263 = CARTESIAN_POINT ( 'NONE',  ( 10.92172942406178926, 9.129999999999999005, 7.935100905948385908 ) ) ;
#4264 = EDGE_LOOP ( 'NONE', ( #10641, #17272, #12349, #9847 ) ) ;
#4265 = CARTESIAN_POINT ( 'NONE',  ( -8.671810352671009525, 43.51358743475483237, -10.34650997788421378 ) ) ;
#4266 = CARTESIAN_POINT ( 'NONE',  ( -7.500000000000000000, 107.5003227710673315, -6.479247348114220983 ) ) ;
#4267 = CARTESIAN_POINT ( 'NONE',  ( 13.42672319008129733, 60.48085777008815711, -1.461561770537686655 ) ) ;
#4268 = CARTESIAN_POINT ( 'NONE',  ( 13.49999999999999822, 7.279999999999994031, 4.386415899144237684 ) ) ;
#4269 = CARTESIAN_POINT ( 'NONE',  ( 0.000000000000000000, 75.00000000000000000, 0.000000000000000000 ) ) ;
#4270 = CARTESIAN_POINT ( 'NONE',  ( 13.47174093492468572, 66.39920212035603697, 0.8849161873603186290 ) ) ;
#4271 = CARTESIAN_POINT ( 'NONE',  ( 3.251687347492562274, 56.79691776447067042, 13.10253915792208090 ) ) ;
#4272 = EDGE_CURVE ( 'NONE', #14369, #10721, #3571, .T. ) ;
#4273 = CARTESIAN_POINT ( 'NONE',  ( 3.636496289402154414, 57.82999999999999829, 11.19198476289190936 ) ) ;
#4274 = CARTESIAN_POINT ( 'NONE',  ( 9.520470885617717371, 64.72999999999998977, -6.917026985038131848 ) ) ;
#4275 = CARTESIAN_POINT ( 'NONE',  ( -12.19111560182831688, 47.14291408922787951, 5.800482751556255145 ) ) ;
#4276 = FACE_OUTER_BOUND ( 'NONE', #5005, .T. ) ;
#4277 = CARTESIAN_POINT ( 'NONE',  ( -19.29752010712827826, 5.918584287042170544, -17.42428528562878398 ) ) ;
#4278 = CARTESIAN_POINT ( 'NONE',  ( 10.50560174212768239, 30.75358953031270204, -8.478557939404936405 ) ) ;
#4279 = CARTESIAN_POINT ( 'NONE',  ( -1.773934221698072244, 56.61635730958409596, 13.38478979355031662 ) ) ;
#4280 = CARTESIAN_POINT ( 'NONE',  ( -11.37499999999960387, -73.88437499999982094, -4.711679271994910323 ) ) ;
#4281 = CARTESIAN_POINT ( 'NONE',  ( 4.171729424061791924, 7.030000000000008242, -12.83926296998457239 ) ) ;
#4282 = CARTESIAN_POINT ( 'NONE',  ( 13.32051220209429054, 33.35292530209495965, 2.195222926766236871 ) ) ;
#4283 = CARTESIAN_POINT ( 'NONE',  ( -10.99999999999979394, 7.773118517290098950, -15.58845726812003996 ) ) ;
#4284 = CARTESIAN_POINT ( 'NONE',  ( 0.000000000000000000, 9.999999999999998224, 0.000000000000000000 ) ) ;
#4285 = CARTESIAN_POINT ( 'NONE',  ( 7.272992578804308828, 22.98000000000001108, 10.01041549318726709 ) ) ;
#4286 = ORIENTED_EDGE ( 'NONE', *, *, #13269, .F. ) ;
#4287 = CARTESIAN_POINT ( 'NONE',  ( -7.499999999999996447, -18.00000000000000355, -2.204364238465235822E-15 ) ) ;
#4288 = EDGE_LOOP ( 'NONE', ( #10045, #3409, #1423, #7450 ) ) ;
#4289 = CARTESIAN_POINT ( 'NONE',  ( 3.636496289402157078, -14.96999999999999709, -11.19198476289190936 ) ) ;
#4290 = CARTESIAN_POINT ( 'NONE',  ( 7.714727599200456254, -60.32187499999988489, -18.62499999999935341 ) ) ;
#4291 = CARTESIAN_POINT ( 'NONE',  ( -13.47250643389561731, 43.90011943282842566, -0.8628561982218695414 ) ) ;
#4292 = CARTESIAN_POINT ( 'NONE',  ( 2.445080149700053643E-15, 1.180000000000002602, -13.50000000000000000 ) ) ;
#4293 = CARTESIAN_POINT ( 'NONE',  ( -13.50000000000000000, 34.92999999999999261, -3.306546357697853733E-15 ) ) ;
#4294 = EDGE_CURVE ( 'NONE', #5101, #13300, #2700, .T. ) ;
#4295 = CARTESIAN_POINT ( 'NONE',  ( 18.62499999999935341, -8.359374999999960920, 7.714727599200469577 ) ) ;
#4296 = CARTESIAN_POINT ( 'NONE',  ( -10.73144679257710443, 67.61893913152461266, -8.194928624396487393 ) ) ;
#4297 = CARTESIAN_POINT ( 'NONE',  ( 13.16986379959833897, -40.61874999999988489, 13.16986379960055409 ) ) ;
#4298 = AXIS2_PLACEMENT_3D ( 'NONE', #3314, #6162, #13038 ) ;
#4299 = CARTESIAN_POINT ( 'NONE',  ( 13.19823589370220418, 54.32922229573070894, 2.848376102529405873 ) ) ;
#4300 = CARTESIAN_POINT ( 'NONE',  ( -10.30332649398041589, 64.59537434288125723, -8.723052715348487141 ) ) ;
#4301 = ORIENTED_EDGE ( 'NONE', *, *, #17013, .F. ) ;
#4302 = CARTESIAN_POINT ( 'NONE',  ( -13.33433074695494902, 35.00395194388527642, 2.108614894658309868 ) ) ;
#4303 = VERTEX_POINT ( 'NONE', #2322 ) ;
#4304 = CARTESIAN_POINT ( 'NONE',  ( 13.40182142610995264, 78.37333532350689325, 1.625185903533163501 ) ) ;
#4305 = DIRECTION ( 'NONE',  ( 1.000000000000000000, 0.000000000000000000, 0.000000000000000000 ) ) ;
#4306 = CARTESIAN_POINT ( 'NONE',  ( -10.92172942406179104, 37.22999999999999687, 7.935100905948387684 ) ) ;
#4307 = CARTESIAN_POINT ( 'NONE',  ( 9.054673339175000280, 72.82854102722255618, -10.02701106865682945 ) ) ;
#4308 = CARTESIAN_POINT ( 'NONE',  ( 6.571298569607622042, 59.92192712267667076, 11.79271934300702895 ) ) ;
#4309 = CARTESIAN_POINT ( 'NONE',  ( 13.49999999999999822, -19.72000000000000597, 4.386415899144237684 ) ) ;
#4310 = CARTESIAN_POINT ( 'NONE',  ( -8.343458848123576743, 61.47999999999999687, -11.48378591275254301 ) ) ;
#4311 = CARTESIAN_POINT ( 'NONE',  ( -11.22131014912690539, 52.64801998336128008, -7.505488620872328376 ) ) ;
#4312 = AXIS2_PLACEMENT_3D ( 'NONE', #9606, #14958, #7121 ) ;
#4313 = ADVANCED_FACE ( 'NONE', ( #2492 ), #7749, .F. ) ;
#4314 = CARTESIAN_POINT ( 'NONE',  ( -9.520470885617715595, 35.62999999999999545, -6.917026985038136289 ) ) ;
#4315 = CARTESIAN_POINT ( 'NONE',  ( 13.50000000000000000, 62.42999999999999972, 1.653273178848926867E-15 ) ) ;
#4316 = CARTESIAN_POINT ( 'NONE',  ( 1.538791601217685434, 50.73532928937410702, 13.41201501813375785 ) ) ;
#4317 = CARTESIAN_POINT ( 'NONE',  ( 10.73231909348931623, 69.11905621171094083, 8.192208697413700946 ) ) ;
#4318 = CARTESIAN_POINT ( 'NONE',  ( -3.763716488224063461, 37.31531146090827633, -12.96716657343995927 ) ) ;
#4319 = CARTESIAN_POINT ( 'NONE',  ( 9.708203932499369415, 4.996025403784432939, 7.053423027509680310 ) ) ;
#4320 = CARTESIAN_POINT ( 'NONE',  ( 13.16986379960055409, -59.28124999999987921, -13.16986379959834430 ) ) ;
#4321 = CARTESIAN_POINT ( 'NONE',  ( -13.25722080889316956, 74.02023315977538687, 2.559143689761975704 ) ) ;
#4322 = SHAPE_REPRESENTATION ( 'Spring', ( #16654 ), #7660 ) ;
#4323 = CARTESIAN_POINT ( 'NONE',  ( -4.728261339063823065, 76.35029506892772133, -12.64499010195072515 ) ) ;
#4324 = AXIS2_PLACEMENT_3D ( 'NONE', #13601, #5321, #1496 ) ;
#4325 = CARTESIAN_POINT ( 'NONE',  ( -12.86241927028127385, 0.1170935115772343549, 5.263970488369911216 ) ) ;
#4326 = DIRECTION ( 'NONE',  ( 0.000000000000000000, 0.000000000000000000, -1.000000000000000000 ) ) ;
#4327 = CARTESIAN_POINT ( 'NONE',  ( -10.98210873310329028, 80.93000000000000682, 5.183560256204878591 ) ) ;
#4328 = CARTESIAN_POINT ( 'NONE',  ( 13.49999999999999822, 31.28000000000000824, 4.386415899144237684 ) ) ;
#4329 = CARTESIAN_POINT ( 'NONE',  ( 11.76794919243112325, -6.720000000000000639, 3.823638476888996163 ) ) ;
#4330 = CARTESIAN_POINT ( 'NONE',  ( -3.636496289402155746, 45.53000000000000114, 11.19198476289190936 ) ) ;
#4331 = CARTESIAN_POINT ( 'NONE',  ( -13.50000000000000000, 1.930000000000015037, -3.469446951953614189E-15 ) ) ;
#4332 = CARTESIAN_POINT ( 'NONE',  ( 7.999999999999850786, 5.918584287042170544, 24.73863375370601858 ) ) ;
#4333 = CARTESIAN_POINT ( 'NONE',  ( 12.24585265403194256, 75.22174939294195894, 5.682387988859129102 ) ) ;
#4334 = CARTESIAN_POINT ( 'NONE',  ( 7.799367850303418948, -7.609836600491641030E-16, -9.406362677511159731 ) ) ;
#4335 = DIRECTION ( 'NONE',  ( 0.000000000000000000, 0.000000000000000000, 1.000000000000000000 ) ) ;
#4336 = CARTESIAN_POINT ( 'NONE',  ( -12.55122207835515447, 41.11055379480070826, 4.971617317440445660 ) ) ;
#4337 = CARTESIAN_POINT ( 'NONE',  ( 4.734980970745145790, 52.00945447310526504, -12.64239079011760403 ) ) ;
#4338 = CARTESIAN_POINT ( 'NONE',  ( -2.901612525891934080, 38.57569620751132788, 13.19105549594109306 ) ) ;
#4339 = CYLINDRICAL_SURFACE ( 'NONE', #10353, 1.999999999999998224 ) ;
#4340 = CARTESIAN_POINT ( 'NONE',  ( -13.49999999999999822, 5.080000000000005400, 4.386415899144235020 ) ) ;
#4341 = CARTESIAN_POINT ( 'NONE',  ( -12.00000000000002842, 0.9139745962155733094, -3.899036354794888304 ) ) ;
#4342 = CARTESIAN_POINT ( 'NONE',  ( -7.375934228542610605, 49.45559395763999078, -11.30689537173397596 ) ) ;
#4343 = CARTESIAN_POINT ( 'NONE',  ( 9.615610945565020273, 63.05944476093819162, 9.475759931419338145 ) ) ;
#4344 = CARTESIAN_POINT ( 'NONE',  ( 13.47794799030919677, 42.40337696373789811, 0.7719109943771497173 ) ) ;
#4345 = CARTESIAN_POINT ( 'NONE',  ( -18.85009555739750198, 7.815224737767797691, 1.645503437279392855 ) ) ;
#4346 = EDGE_CURVE ( 'NONE', #4960, #2740, #13211, .T. ) ;
#4347 = ORIENTED_EDGE ( 'NONE', *, *, #773, .T. ) ;
#4348 = CARTESIAN_POINT ( 'NONE',  ( -3.636496289402155746, 78.53000000000000114, 11.19198476289190936 ) ) ;
#4349 = FACE_OUTER_BOUND ( 'NONE', #9451, .T. ) ;
#4350 = CARTESIAN_POINT ( 'NONE',  ( -11.37500000000039613, -42.66562499999989200, 4.711679271993001628 ) ) ;
#4351 = CARTESIAN_POINT ( 'NONE',  ( 2.621994543952811015E-15, 7.179999999999997939, -14.19474002721660355 ) ) ;
#4352 = VERTEX_POINT ( 'NONE', #15667 ) ;
#4353 = CARTESIAN_POINT ( 'NONE',  ( -8.581213741271680462, 43.50935130007908924, -10.42230493472992414 ) ) ;
#4354 = CARTESIAN_POINT ( 'NONE',  ( -7.499999999999999112, 108.1112172271399885, -5.064597142177449385 ) ) ;
#4355 = CARTESIAN_POINT ( 'NONE',  ( 10.53104951465778072, 60.75217764884847327, -8.446732320805995897 ) ) ;
#4356 = CARTESIAN_POINT ( 'NONE',  ( 4.171729424061791924, 2.030000000000003801, -12.83926296998457239 ) ) ;
#4357 = DIRECTION ( 'NONE',  ( 0.000000000000000000, -1.000000000000000000, 0.000000000000000000 ) ) ;
#4358 = CARTESIAN_POINT ( 'NONE',  ( 11.56614369255154884, 66.68953821447213670, -6.962363570687350567 ) ) ;
#4359 = CARTESIAN_POINT ( 'NONE',  ( 0.9172422442983635404, 56.71299257732687948, 13.47663206627262866 ) ) ;
#4360 = CARTESIAN_POINT ( 'NONE',  ( 3.636496289402154414, 54.83000000000000540, 11.19198476289190936 ) ) ;
#4361 = CARTESIAN_POINT ( 'NONE',  ( -7.576616670048093940E-16, 63.67999999999997840, 12.37355403259654985 ) ) ;
#4362 = CARTESIAN_POINT ( 'NONE',  ( -13.31335613090667636, 46.85142544004738596, -2.237095574266806164 ) ) ;
#4363 = B_SPLINE_CURVE_WITH_KNOTS ( 'NONE', 3,
 ( #685, #6260, #6098, #16854, #10162, #15511, #14359, #8839, #11647, #4928, #14196, #7327, #2078, #10329, #11732, #16016, #15683, #7503 ),
 .UNSPECIFIED., .F., .F.,
 ( 4, 2, 2, 2, 2, 2, 2, 2, 4 ),
 ( 2.344023999658286050E-07, 0.0005273255500080976975, 0.001054416697616229618, 0.001581507845224361646, 0.002108598992832493458, 0.002635690140440625270, 0.003162781288048757081, 0.003689872435656888026, 0.004216963583265019404 ),
 .UNSPECIFIED. ) ;
#4364 = CARTESIAN_POINT ( 'NONE',  ( 13.11257284244564758, 45.54411236249859485, -3.211077615855648659 ) ) ;
#4365 = DIRECTION ( 'NONE',  ( 0.000000000000000000, -1.000000000000000000, 0.000000000000000000 ) ) ;
#4366 = B_SPLINE_CURVE_WITH_KNOTS ( 'NONE', 3,
 ( #2401, #14691, #1096, #13377, #17267, #5179, #1185, #6595, #11975, #3925, #2578, #1266, #4190, #15123, #14859, #8362, #11003, #16374, #9514, #5622, #9689, #12504, #8186, #13719, #476, #9603, #3021, #2754 ),
 .UNSPECIFIED., .F., .F.,
 ( 4, 2, 2, 2, 2, 2, 2, 2, 2, 2, 2, 2, 2, 4 ),
 ( 8.328931132934574426E-17, 0.002882167905697472030, 0.004323251858546166629, 0.005764335811394859926, 0.008646503717092248256, 0.01008758766994094329, 0.01152867162278963659, 0.01296975557563833509, 0.01441083952848702665, 0.01729300743418441325, 0.01873409138703310481, 0.02017517533988179290, 0.02161625929273048100, 0.02305734324557916909 ),
 .UNSPECIFIED. ) ;
#4367 = CARTESIAN_POINT ( 'NONE',  ( 11.52463669016155023, 30.69249958188942173, -7.032419985331740619 ) ) ;
#4368 = CARTESIAN_POINT ( 'NONE',  ( -8.872232410392204116, 56.33699134164967859, 10.17624346630946164 ) ) ;
#4369 = CARTESIAN_POINT ( 'NONE',  ( -4.711679271994916540, -44.74687499999989626, 11.37499999999960210 ) ) ;
#4370 = FACE_OUTER_BOUND ( 'NONE', #6840, .T. ) ;
#4371 = CLOSED_SHELL ( 'NONE', ( #8446, #12472, #17195, #9573, #3177, #5585, #9260, #7781, #16869, #15779, #7854, #1997, #8526, #17373, #2752, #15722, #10424, #12008, #6918, #11838, #8321, #6145, #6164, #98, #404, #5607, #14720, #8358, #3333, #12597, #1565, #6899, #951, #5287, #1688, #4313, #12985, #9740, #16893, #16293, #3523, #6753, #14861, #1613, #5134, #14745, #4225, #15658, #13386, #14527, #13034, #1207, #1883, #7395, #9, #5266, #7953, #2446, #4389, #4090, #15287, #1298, #8860, #14428, #12556, #5159, #17152, #6876, #7192, #11660, #355, #1341, #14050, #810, #3055 ) ) ;
#4372 = CARTESIAN_POINT ( 'NONE',  ( 4.044151295397504953, 32.82541237245334997, 12.88009870303249649 ) ) ;
#4373 = DIRECTION ( 'NONE',  ( 1.182917971378672060E-16, -0.2588190451025143002, 0.9659258262890700886 ) ) ;
#4374 = CARTESIAN_POINT ( 'NONE',  ( 4.326427921100060026, 40.02441582939385256, -12.78796848161989530 ) ) ;
#4375 = EDGE_CURVE ( 'NONE', #13131, #6792, #923, .T. ) ;
#4376 = ORIENTED_EDGE ( 'NONE', *, *, #16117, .T. ) ;
#4377 = CARTESIAN_POINT ( 'NONE',  ( -3.904307695423253843, 62.53961551243608596, 12.92310544161152208 ) ) ;
#4378 = ORIENTED_EDGE ( 'NONE', *, *, #7024, .F. ) ;
#4379 = CARTESIAN_POINT ( 'NONE',  ( -9.520470885617717371, -16.76999999999999957, 6.917026985038133624 ) ) ;
#4380 = CARTESIAN_POINT ( 'NONE',  ( 13.16986379959833897, -71.76874999999985505, 13.16986379960055409 ) ) ;
#4381 = CARTESIAN_POINT ( 'NONE',  ( -13.39575438633939974, 43.86970701691569730, -1.729825961451170180 ) ) ;
#4382 = FACE_OUTER_BOUND ( 'NONE', #9066, .T. ) ;
#4383 = CARTESIAN_POINT ( 'NONE',  ( 13.50000000000000000, 30.42999999999999972, 1.653273178848926867E-15 ) ) ;
#4384 = CARTESIAN_POINT ( 'NONE',  ( -6.062686308920030243, 46.40130649435582910, -12.06266578976461368 ) ) ;
#4385 = CARTESIAN_POINT ( 'NONE',  ( -5.384922564330007155, 67.37499116741884109, -12.38015867815493820 ) ) ;
#4386 = CARTESIAN_POINT ( 'NONE',  ( 18.62500000000000000, -59.34999999999983800, 1.560692158462880521E-12 ) ) ;
#4387 = CARTESIAN_POINT ( 'NONE',  ( 12.98213763223733430, 54.56239296006683759, -3.703273827960795295 ) ) ;
#4388 = CARTESIAN_POINT ( 'NONE',  ( -10.73392024359467278, 64.61856367689141223, -8.199116172563279292 ) ) ;
#4389 = ADVANCED_FACE ( 'NONE', ( #6598 ), #3841, .F. ) ;
#4390 = ORIENTED_EDGE ( 'NONE', *, *, #2530, .F. ) ;
#4391 = CARTESIAN_POINT ( 'NONE',  ( 15.31970530204987035, 8.007293614239921808, -9.835827272001340660 ) ) ;
#4392 = CARTESIAN_POINT ( 'NONE',  ( -13.11532218737669275, 34.81618246207430900, -3.203318699896558375 ) ) ;
#4393 = CARTESIAN_POINT ( 'NONE',  ( 11.37500000000039435, -34.34062499999991047, -4.711679271993004292 ) ) ;
#4394 = VERTEX_POINT ( 'NONE', #7838 ) ;
#4395 = CARTESIAN_POINT ( 'NONE',  ( 13.06826610077310669, 78.55061381712845048, -3.386803558175533357 ) ) ;
#4396 = CARTESIAN_POINT ( 'NONE',  ( -10.99999999999979394, 0.000000000000000000, -15.58845726812003996 ) ) ;
#4397 = CARTESIAN_POINT ( 'NONE',  ( 7.500000000000000888, -21.99999999999990052, -9.367496997597653419 ) ) ;
#4398 = CARTESIAN_POINT ( 'NONE',  ( 10.22275275003651807, 72.76898976254949503, -8.817758165833254225 ) ) ;
#4399 = CARTESIAN_POINT ( 'NONE',  ( 4.773719326841550092, 79.00791013106511684, -12.62843301006502195 ) ) ;
#4400 = CARTESIAN_POINT ( 'NONE',  ( -8.343458848123582072, -14.62000000000000277, 11.48378591275254124 ) ) ;
#4401 = AXIS2_PLACEMENT_3D ( 'NONE', #3802, #7968, #12103 ) ;
#4402 = CARTESIAN_POINT ( 'NONE',  ( 8.343458848123578520, 59.97999999999998977, 11.48378591275254124 ) ) ;
#4403 = CARTESIAN_POINT ( 'NONE',  ( -13.45103708625743977, 52.96991811583343690, 1.151443694251493843 ) ) ;
#4404 = CARTESIAN_POINT ( 'NONE',  ( 7.272992578804308828, 42.97999999999998977, 10.01041549318726709 ) ) ;
#4405 = CARTESIAN_POINT ( 'NONE',  ( 5.883989548015875926, -19.07073847365937169, 10.19133431864935879 ) ) ;
#4406 = CARTESIAN_POINT ( 'NONE',  ( -13.50000000000000000, 57.92999999999999972, -3.306546357697853733E-15 ) ) ;
#4407 = DIRECTION ( 'NONE',  ( 0.000000000000000000, 1.000000000000000000, 0.000000000000000000 ) ) ;
#4408 = CARTESIAN_POINT ( 'NONE',  ( 11.76794919243112325, -3.720000000000000195, 3.823638476888996163 ) ) ;
#4409 = CARTESIAN_POINT ( 'NONE',  ( 5.415421185760910028, 68.87609980712950630, 12.37010947186780463 ) ) ;
#4410 = FACE_OUTER_BOUND ( 'NONE', #2452, .T. ) ;
#4411 = DIRECTION ( 'NONE',  ( -0.000000000000000000, -1.000000000000000000, -0.000000000000000000 ) ) ;
#4412 = CARTESIAN_POINT ( 'NONE',  ( 7.714727599197340524, -87.37812499999982663, 18.62500000000063949 ) ) ;
#4413 = CARTESIAN_POINT ( 'NONE',  ( -12.19220406405763590, 73.71653302039153743, -5.818182159799721198 ) ) ;
#4414 = CIRCLE ( 'NONE', #13430, 26.00000000000000355 ) ;
#4415 = CARTESIAN_POINT ( 'NONE',  ( -4.565779138216930377, 76.34430483734830375, -12.70460796047683694 ) ) ;
#4416 = EDGE_CURVE ( 'NONE', #10663, #11531, #6347, .T. ) ;
#4417 = CARTESIAN_POINT ( 'NONE',  ( -12.50000000000000000, 98.93000000000002103, 1.224646799147353059E-15 ) ) ;
#4418 = DIRECTION ( 'NONE',  ( 0.000000000000000000, 1.000000000000000000, 0.000000000000000000 ) ) ;
#4419 = CARTESIAN_POINT ( 'NONE',  ( 2.150159292860174709, 80.93000000000003524, 13.03677673010521687 ) ) ;
#4420 = CARTESIAN_POINT ( 'NONE',  ( 10.92172942406179104, 31.73000000000000753, -7.935100905948385908 ) ) ;
#4421 = CARTESIAN_POINT ( 'NONE',  ( -9.520470885617717371, -10.76999999999999424, 6.917026985038133624 ) ) ;
#4422 = CARTESIAN_POINT ( 'NONE',  ( 2.272985001014427393E-15, 41.17999999999999972, -12.37355403259654807 ) ) ;
#4423 = CARTESIAN_POINT ( 'NONE',  ( 1.876532330890708260E-11, 6.313974596214807278, -12.00000000000000355 ) ) ;
#4424 = CARTESIAN_POINT ( 'NONE',  ( -1.609251342409827590, 32.62215026715757205, 13.40374960566758311 ) ) ;
#4425 = CARTESIAN_POINT ( 'NONE',  ( 11.64814124600084000, 75.17585265429842423, 6.829356019357755159 ) ) ;
#4426 = CARTESIAN_POINT ( 'NONE',  ( 4.464927919665403699, 5.715075095792275554E-16, -15.55360924457959371 ) ) ;
#4427 = AXIS2_PLACEMENT_3D ( 'NONE', #17098, #7489, #3672 ) ;
#4428 = LINE ( 'NONE', #1585, #7937 ) ;
#4429 = CARTESIAN_POINT ( 'NONE',  ( 8.343458848123583849, 80.88000000000000966, -11.48378591275253768 ) ) ;
#4430 = CARTESIAN_POINT ( 'NONE',  ( 7.976956726953756238, 51.87815718135391307, -10.89215259667266622 ) ) ;
#4431 =( BOUNDED_CURVE ( )  B_SPLINE_CURVE ( 2, ( #8865, #14217, #6379, #11762, #2190, #8945, #14133, #4868, #15713, #6466, #10271, #12825, #5047 ),
 .UNSPECIFIED., .F., .F. ) 
 B_SPLINE_CURVE_WITH_KNOTS ( ( 3, 2, 2, 2, 2, 2, 3 ),
 ( 0.4305555555555555247, 0.4333333333333333481, 0.4388888888888888840, 0.4444444444444444198, 0.4500000000000000111, 0.4555555555555555469, 0.4583333333333333148 ),
 .UNSPECIFIED. ) 
 CURVE ( )  GEOMETRIC_REPRESENTATION_ITEM ( )  RATIONAL_B_SPLINE_CURVE ( ( 0.9755282581475768211, 0.9755282581475765991, 1.000000000000000000, 0.9510565162951535312, 1.000000000000000000, 0.9510565162951535312, 1.000000000000000000, 0.9510565162951535312, 1.000000000000000000, 0.9510565162951535312, 1.000000000000000000, 0.9755282581475770431, 0.9755282581475768211 ) ) 
 REPRESENTATION_ITEM ( '' )  );
#4432 = LINE ( 'NONE', #12382, #11826 ) ;
#4433 = CARTESIAN_POINT ( 'NONE',  ( 5.716269257680778537, 36.97215740540831064, -12.23006940680748933 ) ) ;
#4434 = CARTESIAN_POINT ( 'NONE',  ( -10.92172942406179104, 58.23000000000000398, 7.935100905948387684 ) ) ;
#4435 = CARTESIAN_POINT ( 'NONE',  ( -1.376415865686975826, 49.22940551379771534, -13.43194262913766579 ) ) ;
#4436 = CARTESIAN_POINT ( 'NONE',  ( 11.18930872728590842, 63.14597851813704210, 7.560098781496484399 ) ) ;
#4437 = CARTESIAN_POINT ( 'NONE',  ( 13.48225451615983772, 42.40611353782374948, 0.6920966954215841405 ) ) ;
#4438 = CARTESIAN_POINT ( 'NONE',  ( 7.427339947964860301, 48.90222951860057066, -11.27838517315750799 ) ) ;
#4439 = CARTESIAN_POINT ( 'NONE',  ( -9.520470885617717371, 22.23000000000000043, 6.917026985038133624 ) ) ;
#4440 = ORIENTED_EDGE ( 'NONE', *, *, #15340, .F. ) ;
#4441 = CARTESIAN_POINT ( 'NONE',  ( -11.76794919243112325, 69.07999999999999829, 3.823638476888994830 ) ) ;
#4442 = CARTESIAN_POINT ( 'NONE',  ( -1.900613283894436512, 4.469143981464173798, 12.00000000000000000 ) ) ;
#4443 = CARTESIAN_POINT ( 'NONE',  ( 8.043339635996300530, -64.51874999999984084, 8.043339635997654113 ) ) ;
#4444 = CARTESIAN_POINT ( 'NONE',  ( 10.92172942406179104, 6.730000000000013749, -7.935100905948385908 ) ) ;
#4445 = ORIENTED_EDGE ( 'NONE', *, *, #16392, .T. ) ;
#4446 = CARTESIAN_POINT ( 'NONE',  ( -4.805598482947267769, 43.35318775884549325, -12.61785274320682149 ) ) ;
#4447 = CARTESIAN_POINT ( 'NONE',  ( -7.499999999999998224, 108.7391404411723244, 0.5315352956498785586 ) ) ;
#4448 = CARTESIAN_POINT ( 'NONE',  ( 8.246934402308351508, 60.86644310941438363, -10.69753009404646704 ) ) ;
#4449 = CARTESIAN_POINT ( 'NONE',  ( 13.50000000000000355, 1.579999999999999405, -4.386415899144233244 ) ) ;
#4450 = CARTESIAN_POINT ( 'NONE',  ( -13.16986379959834252, -6.243749999999985256, -13.16986379960055054 ) ) ;
#4451 = CARTESIAN_POINT ( 'NONE',  ( 9.297651317836157503, 66.04322071083470291, 9.806469248494018132 ) ) ;
#4452 = CARTESIAN_POINT ( 'NONE',  ( 5.359754162089569007, 56.87398751003383524, 12.39402400664639003 ) ) ;
#4453 = CARTESIAN_POINT ( 'NONE',  ( 9.520470885617717371, 61.72999999999999687, -6.917026985038131848 ) ) ;
#4454 = CARTESIAN_POINT ( 'NONE',  ( 3.636496289402154414, 69.82999999999999829, 11.19198476289190936 ) ) ;
#4455 = CARTESIAN_POINT ( 'NONE',  ( -12.45694272784634471, 46.74046472961560994, -5.203717773247669598 ) ) ;
#4456 = EDGE_CURVE ( 'NONE', #9433, #4352, #9807, .T. ) ;
#4457 = CARTESIAN_POINT ( 'NONE',  ( 10.24454763814321190, 45.76800118563600250, -8.800910918144792205 ) ) ;
#4458 = CARTESIAN_POINT ( 'NONE',  ( 3.708203932499387179, 7.963974596215601665, 11.41267819554190055 ) ) ;
#4459 = CARTESIAN_POINT ( 'NONE',  ( 24.73863375370598305, 0.000000000000000000, -7.999999999999934275 ) ) ;
#4460 = CARTESIAN_POINT ( 'NONE',  ( 8.403316352008756596, 30.85885728073062140, -10.56577960906128055 ) ) ;
#4461 = CARTESIAN_POINT ( 'NONE',  ( -8.574071495653086572, 56.35097050867326374, 10.42766517367652312 ) ) ;
#4462 = CARTESIAN_POINT ( 'NONE',  ( 11.37500000000000000, -99.89999999999976410, 9.531744055041752924E-13 ) ) ;
#4463 = CARTESIAN_POINT ( 'NONE',  ( -7.499999999999996447, -22.00000000000000000, -9.367496997597603681 ) ) ;
#4464 = CARTESIAN_POINT ( 'NONE',  ( 12.13288869186091645, 33.20991524044760013, 5.984383512105693192 ) ) ;
#4465 = LINE ( 'NONE', #13810, #11372 ) ;
#4466 = CARTESIAN_POINT ( 'NONE',  ( 4.433426395804998421, 40.02052604634783251, -12.75131370640142059 ) ) ;
#4467 = CARTESIAN_POINT ( 'NONE',  ( -3.636496289402156190, 25.52999999999999758, 11.19198476289190758 ) ) ;
#4468 = ORIENTED_EDGE ( 'NONE', *, *, #10645, .T. ) ;
#4469 = CARTESIAN_POINT ( 'NONE',  ( -12.73589991630869100, 62.09160515021331861, 4.477510439207101456 ) ) ;
#4470 = EDGE_LOOP ( 'NONE', ( #10849, #2495, #13382, #8806, #17363 ) ) ;
#4471 = CARTESIAN_POINT ( 'NONE',  ( 11.76794919243112325, -15.57000000000000028, 1.734723475976807094E-15 ) ) ;
#4472 = CARTESIAN_POINT ( 'NONE',  ( 18.62500000000064659, -58.24062499999988063, -7.714727599197336083 ) ) ;
#4473 = CARTESIAN_POINT ( 'NONE',  ( -12.73615524967575574, 43.76842681669471347, -4.476659004287373733 ) ) ;
#4474 = CARTESIAN_POINT ( 'NONE',  ( 13.49999999999999822, 0.2799999999999969180, 4.386415899144236796 ) ) ;
#4475 = CARTESIAN_POINT ( 'NONE',  ( -4.171729424061787483, 34.32999999999999829, -12.83926296998457417 ) ) ;
#4476 = CARTESIAN_POINT ( 'NONE',  ( -8.343458848123582072, 46.37999999999999545, 11.48378591275254124 ) ) ;
#4477 = CARTESIAN_POINT ( 'NONE',  ( -1.937690227285938205, 46.24965744208711982, -13.36137179930980778 ) ) ;
#4478 = CARTESIAN_POINT ( 'NONE',  ( -2.917897579637011241, 67.28493650261737002, -13.18089723172849403 ) ) ;
#4479 = CARTESIAN_POINT ( 'NONE',  ( -18.62500000000000000, -67.67499999999981242, -1.562973063126292757E-12 ) ) ;
#4480 = CARTESIAN_POINT ( 'NONE',  ( 10.76214398255494586, 54.12080488597943173, 8.150716040728196887 ) ) ;
#4481 = CARTESIAN_POINT ( 'NONE',  ( -0.4982172014182387754, 64.19791404813746283, -13.49082082228690638 ) ) ;
#4482 = VERTEX_POINT ( 'NONE', #13040 ) ;
#4483 = CARTESIAN_POINT ( 'NONE',  ( -10.04923048958269405, 34.58189789653238932, -9.015230755480622804 ) ) ;
#4484 = CARTESIAN_POINT ( 'NONE',  ( -8.043339635997654113, -10.40624999999997513, 8.043339635996302306 ) ) ;
#4485 = CARTESIAN_POINT ( 'NONE',  ( 13.40746492369621556, 78.48656952345000093, -1.623796509401284283 ) ) ;
#4486 = CARTESIAN_POINT ( 'NONE',  ( 0.000000000000000000, 5.918584287042170544, 0.000000000000000000 ) ) ;
#4487 = CARTESIAN_POINT ( 'NONE',  ( 7.500000000000001776, -23.27245777243038916, -9.199283337799341709 ) ) ;
#4488 = CARTESIAN_POINT ( 'NONE',  ( 12.96587728178895738, 72.56450825003899752, -3.759848239116166280 ) ) ;
#4489 = CARTESIAN_POINT ( 'NONE',  ( 10.92172942406178926, -16.86999999999999744, 7.935100905948385908 ) ) ;
#4490 = CARTESIAN_POINT ( 'NONE',  ( -10.92172942406179104, 59.22999999999999687, 7.935100905948387684 ) ) ;
#4491 = CARTESIAN_POINT ( 'NONE',  ( -1.175964444707957579, 71.63773400114577328, 13.45120314782261772 ) ) ;
#4492 = EDGE_CURVE ( 'NONE', #17443, #12574, #12063, .T. ) ;
#4493 = CARTESIAN_POINT ( 'NONE',  ( -11.76794919243112325, 35.92999999999999972, -2.882316262207890869E-15 ) ) ;
#4494 = CARTESIAN_POINT ( 'NONE',  ( -8.343458848123576743, 54.48000000000000398, -11.48378591275254301 ) ) ;
#4495 = EDGE_CURVE ( 'NONE', #6493, #13300, #16020, .T. ) ;
#4496 = DIRECTION ( 'NONE',  ( -0.000000000000000000, 1.000000000000000000, -0.000000000000000000 ) ) ;
#4497=STYLED_ITEM('',(#17519),#8814);
#4498 = CARTESIAN_POINT ( 'NONE',  ( 11.76794919243112680, -3.420000000000002593, -3.823638476888993942 ) ) ;
#4499 = CARTESIAN_POINT ( 'NONE',  ( 10.86192711411459122, 69.12653421500604622, 8.016776366340984339 ) ) ;
#4500 = CARTESIAN_POINT ( 'NONE',  ( 12.00000000000002665, 2.563974596215591983, 1.734723475976807094E-15 ) ) ;
#4501 = CARTESIAN_POINT ( 'NONE',  ( -2.138189944381230223, 73.60311857767972299, 13.50000000000000178 ) ) ;
#4502 = CARTESIAN_POINT ( 'NONE',  ( -18.62499999999935341, -81.13437499999982094, -7.714727599200458030 ) ) ;
#4503 = CARTESIAN_POINT ( 'NONE',  ( -11.39092472967678837, 73.65879597142989610, -7.245477644767023939 ) ) ;
#4504 = CARTESIAN_POINT ( 'NONE',  ( -2.389462197225028728, 76.26591624804247260, -13.28685410492694530 ) ) ;
#4505 = CARTESIAN_POINT ( 'NONE',  ( -2.138187132794193701, 0.6031186787740299149, 13.50000091354000809 ) ) ;
#4506 = CARTESIAN_POINT ( 'NONE',  ( -7.416407864998736166, 0.3460254037844350261, -10.20780970022448031 ) ) ;
#4507 = CARTESIAN_POINT ( 'NONE',  ( -1.003751346110120011E-07, 3.679997203684337137, 13.49999999999999822 ) ) ;
#4508 = CARTESIAN_POINT ( 'NONE',  ( -4.171729424061787483, 29.32999999999999474, -12.83926296998457417 ) ) ;
#4509 = CARTESIAN_POINT ( 'NONE',  ( 11.76794919243112325, -9.569999999999994955, 1.734723475976807094E-15 ) ) ;
#4510 = CARTESIAN_POINT ( 'NONE',  ( -3.636496289402153081, 35.32999999999999829, -11.19198476289190936 ) ) ;
#4511 = CARTESIAN_POINT ( 'NONE',  ( 7.999999999999868550, 6.548268786306342903, 22.26879735319531761 ) ) ;
#4512 = CARTESIAN_POINT ( 'NONE',  ( 8.311262620771346477, 74.99693123154169427, 10.63835658022000707 ) ) ;
#4513 = CARTESIAN_POINT ( 'NONE',  ( 18.62500000000000000, 0.000000000000000000, 1.560692158462880521E-12 ) ) ;
#4514 = CARTESIAN_POINT ( 'NONE',  ( 9.520470885617717371, 34.72999999999999687, -6.917026985038131848 ) ) ;
#4515 = CARTESIAN_POINT ( 'NONE',  ( -9.520470885617715595, 32.63000000000000256, -6.917026985038136289 ) ) ;
#4516 = EDGE_CURVE ( 'NONE', #14499, #16836, #6691, .T. ) ;
#4517 = CARTESIAN_POINT ( 'NONE',  ( 4.761726286637288474, 52.00846422156020310, -12.63236328405458408 ) ) ;
#4518 = CARTESIAN_POINT ( 'NONE',  ( -1.596087918524577542, 38.62259808071801359, 13.40533364316977760 ) ) ;
#4519 = LINE ( 'NONE', #5943, #17106 ) ;
#4520 = CARTESIAN_POINT ( 'NONE',  ( -17.32050807568867512, 0.000000000000000000, -8.000000000000207834 ) ) ;
#4521 = CARTESIAN_POINT ( 'NONE',  ( -2.559407043143859806, 49.27189254790160788, -13.26134293993454705 ) ) ;
#4522 = CARTESIAN_POINT ( 'NONE',  ( 4.408271315188386552, 62.83777092602397829, 12.79017921344417097 ) ) ;
#4523 = CARTESIAN_POINT ( 'NONE',  ( 13.32680416487845321, 42.35436111799107550, 2.155617169667197963 ) ) ;
#4524 = CARTESIAN_POINT ( 'NONE',  ( 8.550215766970532982, 48.85207767227580433, -10.44719490448041022 ) ) ;
#4525 = CARTESIAN_POINT ( 'NONE',  ( -11.76794919243112325, 18.78000000000001180, -3.823638476888998827 ) ) ;
#4526 = VERTEX_POINT ( 'NONE', #9344 ) ;
#4527 = CARTESIAN_POINT ( 'NONE',  ( -3.636496289402153081, 68.32999999999999829, -11.19198476289190936 ) ) ;
#4528 = CARTESIAN_POINT ( 'NONE',  ( -7.714727599200466912, -87.44687499999976410, 18.62499999999935341 ) ) ;
#4529 = CARTESIAN_POINT ( 'NONE',  ( 8.043339635996300530, -81.16874999999980389, 8.043339635997654113 ) ) ;
#4530 = CARTESIAN_POINT ( 'NONE',  ( -4.171729424061787483, 10.33000000000000540, -12.83926296998457417 ) ) ;
#4531 = ORIENTED_EDGE ( 'NONE', *, *, #11260, .T. ) ;
#4532 = CARTESIAN_POINT ( 'NONE',  ( -0.006952547203360656333, 43.18024923986452279, -13.49999999219945934 ) ) ;
#4533 = CARTESIAN_POINT ( 'NONE',  ( -25.42428528562849266, 5.918584287042170544, -5.441113646577749208 ) ) ;
#4534 = CARTESIAN_POINT ( 'NONE',  ( -8.549982208541774191E-16, 3.680000000000005933, 14.19474002721660355 ) ) ;
#4535 = CARTESIAN_POINT ( 'NONE',  ( 13.16986379960055054, -2.081249999999994937, -13.16986379959834430 ) ) ;
#4536 = CARTESIAN_POINT ( 'NONE',  ( 11.81479127198460155, 66.18791984854836130, 6.531537704173645764 ) ) ;
#4537 = AXIS2_PLACEMENT_3D ( 'NONE', #888, #14146, #11432 ) ;
#4538 = CARTESIAN_POINT ( 'NONE',  ( 8.254427490791934829, 56.99432593801493852, 10.68333636219931293 ) ) ;
#4539 = CARTESIAN_POINT ( 'NONE',  ( -11.76794919243112325, 63.07999999999999119, 3.823638476888994386 ) ) ;
#4540 = CARTESIAN_POINT ( 'NONE',  ( 8.343458848123583849, 32.88000000000000256, -11.48378591275253768 ) ) ;
#4541 = CARTESIAN_POINT ( 'NONE',  ( -3.636496289402155746, 69.53000000000001535, 11.19198476289190936 ) ) ;
#4542 = EDGE_CURVE ( 'NONE', #9435, #7272, #5284, .T. ) ;
#4543 = CARTESIAN_POINT ( 'NONE',  ( -12.56761561834811403, 46.75105081705815735, -4.930021005048375926 ) ) ;
#4544 = CARTESIAN_POINT ( 'NONE',  ( 9.264981600666393646, 45.81801372893175284, -9.819209257909990995 ) ) ;
#4545 = CARTESIAN_POINT ( 'NONE',  ( -7.999999999999670486, 0.000000000000000000, -24.73863375370606477 ) ) ;
#4546 = CARTESIAN_POINT ( 'NONE',  ( 1.732050807568739970, 7.773118517290100726, 19.00000000000000355 ) ) ;
#4547 = CARTESIAN_POINT ( 'NONE',  ( 0.6446146492995459276, 31.15683549778061234, -13.48678750428668494 ) ) ;
#4548 = CARTESIAN_POINT ( 'NONE',  ( -10.17582679281236935, 56.27190818227264657, 8.882075982020387173 ) ) ;
#4549 = DIRECTION ( 'NONE',  ( -3.552713678800500929E-15, 0.000000000000000000, 1.000000000000000000 ) ) ;
#4550 = CARTESIAN_POINT ( 'NONE',  ( 0.9449016496340574278, 32.71398372948575428, 13.46769545381985012 ) ) ;
#4551 = CARTESIAN_POINT ( 'NONE',  ( -10.56248930388449558, 10.00000000000000000, 5.855161195429291254 ) ) ;
#4552 = CARTESIAN_POINT ( 'NONE',  ( 10.54603764524003040, 39.75142172891366954, -8.431702247120188787 ) ) ;
#4553 = CARTESIAN_POINT ( 'NONE',  ( -7.409984580736203970E-16, 25.67999999999999616, 12.37355403259654985 ) ) ;
#4554 = VERTEX_POINT ( 'NONE', #3667 ) ;
#4555 = CARTESIAN_POINT ( 'NONE',  ( -13.46566103132326297, 61.96328914063155224, 0.9623097876522905825 ) ) ;
#4556 = VERTEX_POINT ( 'NONE', #11806 ) ;
#4557 = CARTESIAN_POINT ( 'NONE',  ( -1.564113515457998370E-12, -36.38749999999993179, 18.62500000000000000 ) ) ;
#4558 = CARTESIAN_POINT ( 'NONE',  ( 10.70843530424569856, 48.11775999830372541, 8.220672230353347487 ) ) ;
#4559 = CARTESIAN_POINT ( 'NONE',  ( -8.891200544363830713E-16, 64.67999999999999261, 13.50000000000000000 ) ) ;
#4560 = CARTESIAN_POINT ( 'NONE',  ( -10.92172942406178926, 34.62999999999999545, -7.935100905948389460 ) ) ;
#4561 = CARTESIAN_POINT ( 'NONE',  ( -10.92172942406179104, 40.23000000000000398, 7.935100905948387684 ) ) ;
#4562 = CARTESIAN_POINT ( 'NONE',  ( -2.198120649712783869, 46.25903117140494203, -13.32013477985053918 ) ) ;
#4563 = CARTESIAN_POINT ( 'NONE',  ( -2.264496491277277812, 67.26149511457354890, -13.31769803748488279 ) ) ;
#4564 = CARTESIAN_POINT ( 'NONE',  ( -8.043339635996304082, 1.006250000000015854, -8.043339635997652337 ) ) ;
#4565 = CARTESIAN_POINT ( 'NONE',  ( 6.801677017248844770, 53.93148548877682202, 11.66148778661555951 ) ) ;
#4566 = VERTEX_POINT ( 'NONE', #1098 ) ;
#4567 = CARTESIAN_POINT ( 'NONE',  ( -0.1481528981132104184, 64.18532703164794384, -13.49999999999999645 ) ) ;
#4568 = ORIENTED_EDGE ( 'NONE', *, *, #7589, .T. ) ;
#4569 = AXIS2_PLACEMENT_3D ( 'NONE', #9017, #6365, #1128 ) ;
#4570 = CARTESIAN_POINT ( 'NONE',  ( -8.000000000000145661, 0.000000000000000000, 17.32050807568870709 ) ) ;
#4571 = CARTESIAN_POINT ( 'NONE',  ( -9.956290844395114803, 34.57701004435445924, -9.118751552402068583 ) ) ;
#4572 = CARTESIAN_POINT ( 'NONE',  ( -4.711679271993004292, -71.80312499999982379, -11.37500000000039435 ) ) ;
#4573 = CARTESIAN_POINT ( 'NONE',  ( 13.07345783715813603, 78.54986944972205265, -3.366722508972363581 ) ) ;
#4574 = CARTESIAN_POINT ( 'NONE',  ( -15.43600950528680116, 7.854010657973331533, 10.69176227072916951 ) ) ;
#4575 = PLANE ( 'NONE',  #6498 ) ;
#4576 = CARTESIAN_POINT ( 'NONE',  ( 7.500000000000002665, -22.25853674790688075, -9.367496997597603681 ) ) ;
#4577 = CARTESIAN_POINT ( 'NONE',  ( 13.35802549108727000, 72.36165858179914778, 1.953960687672332108 ) ) ;
#4578 = CARTESIAN_POINT ( 'NONE',  ( -7.272992578804307939, 27.48000000000001108, -10.01041549318726886 ) ) ;
#4579 = CARTESIAN_POINT ( 'NONE',  ( -4.171729424061791036, 65.53000000000000114, 12.83926296998457239 ) ) ;
#4580 = CARTESIAN_POINT ( 'NONE',  ( -8.831087761643750866, 52.52108727616624151, -10.21087246435311435 ) ) ;
#4581 = CARTESIAN_POINT ( 'NONE',  ( -3.636496289402153081, 35.32999999999999829, -11.19198476289190936 ) ) ;
#4582 = CARTESIAN_POINT ( 'NONE',  ( -13.50000000000000000, 54.92999999999999972, -3.306546357697853733E-15 ) ) ;
#4583 = AXIS2_PLACEMENT_3D ( 'NONE', #6540, #6274, #17213 ) ;
#4584 = PLANE ( 'NONE',  #3342 ) ;
#4585 = CARTESIAN_POINT ( 'NONE',  ( -11.76794919243112325, -5.069999999999998508, -2.602085213965210642E-15 ) ) ;
#4586 = CARTESIAN_POINT ( 'NONE',  ( 10.00340607087883349, 69.07939772179537385, 9.065424430625297347 ) ) ;
#4587 = FACE_OUTER_BOUND ( 'NONE', #13999, .T. ) ;
#4588 = B_SPLINE_CURVE_WITH_KNOTS ( 'NONE', 3,
 ( #9693, #9781, #4551, #8278, #1533, #9870, #15220, #6949, #11096, #1793, #15128, #12327, #7039, #7204, #9956, #12590, #479, #5626, #11007, #3209, #1876, #16378, #12417, #12237, #5714, #8887 ),
 .UNSPECIFIED., .F., .F.,
 ( 4, 2, 2, 2, 2, 2, 2, 2, 2, 2, 2, 2, 4 ),
 ( 0.003287795359550850938, 0.004729367074732778939, 0.006170938789914706506, 0.007612510505096635807, 0.009054082220278565976, 0.01193722565064242458, 0.01337879736582435475, 0.01482036908100628665, 0.01626194079618821509, 0.01770351251137014525, 0.02058665594173400559, 0.02346979937209786593, 0.02635294280246172627 ),
 .UNSPECIFIED. ) ;
#4589 = CARTESIAN_POINT ( 'NONE',  ( -7.714727599200466912, -68.64687499999988063, 18.62499999999935341 ) ) ;
#4590 = CARTESIAN_POINT ( 'NONE',  ( -10.86631776481396905, 73.62653164792240545, -8.015947894086419723 ) ) ;
#4591 = CARTESIAN_POINT ( 'NONE',  ( -7.225584998327790665, 76.44917738724952017, -11.40355617289543844 ) ) ;
#4592 = CARTESIAN_POINT ( 'NONE',  ( -10.92172942406179104, 0.2300000000000079758, 7.935100905948385908 ) ) ;
#4593 = CARTESIAN_POINT ( 'NONE',  ( 8.061801495184115041, 7.889711263303322397, -16.81068189100985322 ) ) ;
#4594 = CARTESIAN_POINT ( 'NONE',  ( 13.50000000000000355, 31.57999999999999474, -4.386415899144233244 ) ) ;
#4595 = CARTESIAN_POINT ( 'NONE',  ( 2.279995255611139653E-15, -5.820000000000007390, -12.37355403259654985 ) ) ;
#4596 = EDGE_CURVE ( 'NONE', #19, #902, #5002, .T. ) ;
#4597 = CARTESIAN_POINT ( 'NONE',  ( -11.76794919243112325, 38.92999999999999972, -2.882316262207890869E-15 ) ) ;
#4598 = CARTESIAN_POINT ( 'NONE',  ( 9.708203932499369415, 5.263974596215557966, 7.053423027509680310 ) ) ;
#4599 = CARTESIAN_POINT ( 'NONE',  ( -7.124089981346021005, 32.41512088030167149, 11.46724091227400955 ) ) ;
#4600 = CARTESIAN_POINT ( 'NONE',  ( 4.878482463424276716, 74.85599699807477236, 12.59450660046991999 ) ) ;
#4601 = CARTESIAN_POINT ( 'NONE',  ( 8.343458848123580296, 61.97999999999999687, 11.48378591275253768 ) ) ;
#4602 =( LENGTH_UNIT ( ) NAMED_UNIT ( * ) SI_UNIT ( .MILLI., .METRE. ) );
#4603 = CARTESIAN_POINT ( 'NONE',  ( -10.92172942406179104, 82.23000000000000398, 7.935100905948387684 ) ) ;
#4604 = CARTESIAN_POINT ( 'NONE',  ( 10.04308425913412250, 51.77851858841606969, -9.021445512424994817 ) ) ;
#4605 = CARTESIAN_POINT ( 'NONE',  ( -6.476206340861387467, 38.44199689924342778, 11.84763527750397394 ) ) ;
#4606 = CARTESIAN_POINT ( 'NONE',  ( 8.074219154787348529, 36.87380170060612983, -10.82003361857776547 ) ) ;
#4607 = CARTESIAN_POINT ( 'NONE',  ( 0.000000000000000000, 3.000000000000000000, -5.000000000000000000 ) ) ;
#4608 = CARTESIAN_POINT ( 'NONE',  ( -4.136362903238101296, 49.32872232693532055, -12.85098559761272874 ) ) ;
#4609 = CARTESIAN_POINT ( 'NONE',  ( 2.690935862572700010, 62.77670372775656915, 13.22909870504613927 ) ) ;
#4610 = CARTESIAN_POINT ( 'NONE',  ( -11.76794919243112325, 80.92999999999767624, -5.919446256302011733E-11 ) ) ;
#4611 = CARTESIAN_POINT ( 'NONE',  ( 12.99504019031924962, 48.56107377554576487, -3.664513708583787110 ) ) ;
#4612 = CARTESIAN_POINT ( 'NONE',  ( -3.636496289402152637, 21.33000000000001606, -11.19198476289190936 ) ) ;
#4613 = ORIENTED_EDGE ( 'NONE', *, *, #7633, .T. ) ;
#4614 = CARTESIAN_POINT ( 'NONE',  ( -3.636496289402153081, 65.32999999999999829, -11.19198476289190936 ) ) ;
#4615 = CARTESIAN_POINT ( 'NONE',  ( -9.552639591052204498E-13, -5.237499999999969624, 11.37500000000000178 ) ) ;
#4616 = CARTESIAN_POINT ( 'NONE',  ( 4.711679271994910323, -86.37187499999978968, -11.37499999999960387 ) ) ;
#4617 = CARTESIAN_POINT ( 'NONE',  ( -13.49999999999999822, 5.080000000000005400, 4.386415899144235908 ) ) ;
#4618 = ADVANCED_FACE ( 'NONE', ( #5095 ), #10487, .T. ) ;
#4619 = CARTESIAN_POINT ( 'NONE',  ( -1.849123144677635722, 43.24648372408316277, -13.37408686090705956 ) ) ;
#4620 = CARTESIAN_POINT ( 'NONE',  ( 0.8082646707930503105, 76.15093783529552240, -13.47583662643777913 ) ) ;
#4621 = CARTESIAN_POINT ( 'NONE',  ( -13.49999999999999822, 5.779999999999998472, -4.386415899144240349 ) ) ;
#4622 = CARTESIAN_POINT ( 'NONE',  ( -13.16986379959834252, -39.54374999999990337, -13.16986379960055054 ) ) ;
#4623 = CARTESIAN_POINT ( 'NONE',  ( 5.725467330485540352, 65.88816334722764623, 12.22575439232458727 ) ) ;
#4624 = CARTESIAN_POINT ( 'NONE',  ( -13.50000000000000000, 82.93000000000000682, -3.306546357697853733E-15 ) ) ;
#4625 = CARTESIAN_POINT ( 'NONE',  ( -11.76794919243112325, 54.07999999999999119, 3.823638476888994386 ) ) ;
#4626 = CARTESIAN_POINT ( 'NONE',  ( 2.607531440858944223E-15, 33.17999999999999261, -14.19474002721660355 ) ) ;
#4627 = CARTESIAN_POINT ( 'NONE',  ( -11.76794919243112325, 57.07999999999999829, 3.823638476888994386 ) ) ;
#4628 = CARTESIAN_POINT ( 'NONE',  ( -13.22621774997404920, 47.02780800035617403, 2.761248823199535796 ) ) ;
#4629 = CARTESIAN_POINT ( 'NONE',  ( 9.091354351312018522, 45.82646639924907106, -9.980085113653212048 ) ) ;
#4630 = CARTESIAN_POINT ( 'NONE',  ( 8.426818388819521388, 69.85781622895851228, -10.54854181807195879 ) ) ;
#4631 = CARTESIAN_POINT ( 'NONE',  ( -12.00000000000000178, 6.913974596215557433, -3.899036354794879866 ) ) ;
#4632 = CARTESIAN_POINT ( 'NONE',  ( 10.37303206245883302, 30.76086691204845991, -8.640359589916528193 ) ) ;
#4633 = CARTESIAN_POINT ( 'NONE',  ( -12.38444555254770485, 55.73389167458477544, -5.378193122225002121 ) ) ;
#4634 = CARTESIAN_POINT ( 'NONE',  ( 2.138189944381242213, 54.10311857767973009, -13.49999999999999822 ) ) ;
#4635 = CARTESIAN_POINT ( 'NONE',  ( 7.123395093792429300, 32.94489533744902587, 11.46981911532503240 ) ) ;
#4636 = CARTESIAN_POINT ( 'NONE',  ( 2.911951681939318970, 43.07529696608821723, -13.18220571944093500 ) ) ;
#4637 = CARTESIAN_POINT ( 'NONE',  ( 11.19045305759900089, 39.71388240225230959, -7.551420157137952671 ) ) ;
#4638 = VERTEX_POINT ( 'NONE', #15934 ) ;
#4639 = CARTESIAN_POINT ( 'NONE',  ( -13.22913111164857192, 61.83496861166081260, -2.690993549969627807 ) ) ;
#4640 = VERTEX_POINT ( 'NONE', #2580 ) ;
#4641 = ADVANCED_FACE ( 'NONE', ( #4370 ), #4193, .F. ) ;
#4642 = CARTESIAN_POINT ( 'NONE',  ( 13.50000000000000355, 30.57999999999999829, -4.386415899144233244 ) ) ;
#4643 = CARTESIAN_POINT ( 'NONE',  ( 7.714727599200456254, -93.62187499999978968, -18.62499999999935341 ) ) ;
#4644 =( BOUNDED_CURVE ( )  B_SPLINE_CURVE ( 2, ( #14119, #4941, #16865, #700, #2175, #10342, #6110, #6363, #4770, #3604, #9453 ),
 .UNSPECIFIED., .F., .F. ) 
 B_SPLINE_CURVE_WITH_KNOTS ( ( 3, 2, 2, 2, 2, 3 ),
 ( 0.07409432434525202449, 0.07777777777777777901, 0.08333333333333332871, 0.08888888888888889228, 0.09444444444444444198, 0.09722222222222222376 ),
 .UNSPECIFIED. ) 
 CURVE ( )  GEOMETRIC_REPRESENTATION_ITEM ( )  RATIONAL_B_SPLINE_CURVE ( ( 0.9781297068810623774, 0.9675494122505707839, 1.000000000000000000, 0.9510565162951535312, 1.000000000000000000, 0.9510565162951535312, 1.000000000000000000, 0.9510565162951535312, 1.000000000000000000, 0.9755282581475768211, 0.9755282581475768211 ) ) 
 REPRESENTATION_ITEM ( '' )  );
#4645 = CARTESIAN_POINT ( 'NONE',  ( 2.636941296682203006, 58.08524355054738209, -13.24082347101475321 ) ) ;
#4646 = CARTESIAN_POINT ( 'NONE',  ( -4.171729424061787483, 37.32999999999999829, -12.83926296998457417 ) ) ;
#4647 = CARTESIAN_POINT ( 'NONE',  ( 0.2690821827029589719, 65.68967525039607835, 13.49733241026649821 ) ) ;
#4648 = VECTOR ( 'NONE', #15524, 1000.000000000000000 ) ;
#4649 = CARTESIAN_POINT ( 'NONE',  ( -3.930507969928632939, 46.32123624867764278, -12.91573196151841074 ) ) ;
#4650 = DIRECTION ( 'NONE',  ( 0.000000000000000000, -1.000000000000000000, 0.000000000000000000 ) ) ;
#4651 = CARTESIAN_POINT ( 'NONE',  ( -11.37499999999960743, -33.33437499999990195, -4.711679271994912099 ) ) ;
#4652 = CARTESIAN_POINT ( 'NONE',  ( 11.21398382682447448, 54.14760983389460591, 7.519816583474207228 ) ) ;
#4653 = ORIENTED_EDGE ( 'NONE', *, *, #13992, .F. ) ;
#4654 = CARTESIAN_POINT ( 'NONE',  ( -8.608562527083625682, 64.51060847542233034, -10.40036578628359010 ) ) ;
#4655 = EDGE_LOOP ( 'NONE', ( #12526, #13284, #11422, #2347 ) ) ;
#4656 = CARTESIAN_POINT ( 'NONE',  ( 2.710823146150888707, 67.08252889310698208, -13.22504384347605288 ) ) ;
#4657 = CARTESIAN_POINT ( 'NONE',  ( -10.97982169273876707, 34.63276478775296141, -7.866720829704087592 ) ) ;
#4658 = CARTESIAN_POINT ( 'NONE',  ( -10.92172942406178926, 17.63000000000000611, -7.935100905948389460 ) ) ;
#4659 = CARTESIAN_POINT ( 'NONE',  ( -4.711679271993004292, -38.50312499999991189, -11.37500000000039435 ) ) ;
#4660 = CARTESIAN_POINT ( 'NONE',  ( 7.867868983202085609, 77.97688993890311338, 10.97928513584511911 ) ) ;
#4661 = CARTESIAN_POINT ( 'NONE',  ( 2.445080149700053643E-15, 48.17999999999999972, -13.50000000000000000 ) ) ;
#4662 = LINE ( 'NONE', #15420, #7352 ) ;
#4663 = CARTESIAN_POINT ( 'NONE',  ( 7.500000000000000888, -27.17584396961776250, 5.080312676971243668 ) ) ;
#4664 = CARTESIAN_POINT ( 'NONE',  ( 12.95808625703547001, 72.29434740553908512, 3.790096261879717598 ) ) ;
#4665 = CARTESIAN_POINT ( 'NONE',  ( -9.520470885617717371, 28.23000000000000398, 6.917026985038133624 ) ) ;
#4666 = CARTESIAN_POINT ( 'NONE',  ( -13.49999999999999822, 58.77999999999998693, -4.386415899144240349 ) ) ;
#4667 = CARTESIAN_POINT ( 'NONE',  ( -4.319839466158835073, 52.33534458003789780, -12.79062298228854822 ) ) ;
#4668 = CARTESIAN_POINT ( 'NONE',  ( -11.76794919243112325, 38.77999999999999403, -3.823638476888998827 ) ) ;
#4669 = CARTESIAN_POINT ( 'NONE',  ( -11.76794919243112325, -14.06999999999999851, -2.602085213965210642E-15 ) ) ;
#4670 = CARTESIAN_POINT ( 'NONE',  ( 8.343458848123578520, 58.98000000000000398, 11.48378591275254124 ) ) ;
#4671 = DIRECTION ( 'NONE',  ( -0.4999999999999953371, -0.000000000000000000, -0.8660254037844413721 ) ) ;
#4672 = EDGE_CURVE ( 'NONE', #6684, #4811, #4707, .T. ) ;
#4673 = CARTESIAN_POINT ( 'NONE',  ( 9.520470885617717371, -0.2699999999999924682, -6.917026985038131848 ) ) ;
#4674 = CARTESIAN_POINT ( 'NONE',  ( -0.7780706695535477557, 68.65214339747750216, 13.47801817613818187 ) ) ;
#4675 = CARTESIAN_POINT ( 'NONE',  ( 18.62500000000064304, -34.34062499999991047, -7.714727599197335195 ) ) ;
#4676 = CARTESIAN_POINT ( 'NONE',  ( -13.49999999999999822, 4.780000000000000249, -4.386415899144240349 ) ) ;
#4677 = CARTESIAN_POINT ( 'NONE',  ( -1.564113515457998370E-12, -102.9874999999997698, 18.62500000000000000 ) ) ;
#4678 = CARTESIAN_POINT ( 'NONE',  ( -13.47543018545582072, 73.95811523521949482, 0.8141832615170856435 ) ) ;
#4679 = CARTESIAN_POINT ( 'NONE',  ( -2.366530682011494413, 76.26509166571406695, -13.29096256660020536 ) ) ;
#4680 = LINE ( 'NONE', #8760, #9318 ) ;
#4681 = CARTESIAN_POINT ( 'NONE',  ( 0.000000000000000000, 0.000000000000000000, 0.000000000000000000 ) ) ;
#4682 = CARTESIAN_POINT ( 'NONE',  ( 4.171729424061791924, 26.02999999999999758, -12.83926296998457239 ) ) ;
#4683 = CARTESIAN_POINT ( 'NONE',  ( 7.272992578804311492, -6.120000000000004547, -10.01041549318726709 ) ) ;
#4684 = CARTESIAN_POINT ( 'NONE',  ( -11.76794919243112325, 36.07999999999999829, 3.823638476888994830 ) ) ;
#4685 = CIRCLE ( 'NONE', #11458, 12.00000000000000178 ) ;
#4686 = CARTESIAN_POINT ( 'NONE',  ( 1.469576158976824144E-15, 9.000000000000000000, 12.00000000000000178 ) ) ;
#4687 = CARTESIAN_POINT ( 'NONE',  ( -3.895040229899401574, 32.54007840815446428, 12.92655551793117752 ) ) ;
#4688 = CARTESIAN_POINT ( 'NONE',  ( 7.957144986088850125, 74.98096353892839261, 10.90684177774465624 ) ) ;
#4689 = CARTESIAN_POINT ( 'NONE',  ( -1.003760800223034469E-07, 53.67999720368429450, 13.49999999999999822 ) ) ;
#4690 = CARTESIAN_POINT ( 'NONE',  ( 9.520470885617717371, 31.72999999999999332, -6.917026985038131848 ) ) ;
#4691 = CARTESIAN_POINT ( 'NONE',  ( 11.77278396783205494, 51.67514776089146267, -6.607601308730693290 ) ) ;
#4692 = CARTESIAN_POINT ( 'NONE',  ( -1.732050807568877859, 0.000000000000000000, -18.99999999999999645 ) ) ;
#4693 = CARTESIAN_POINT ( 'NONE',  ( 1.203083463835363736E-13, 37.18000000000000682, -13.50000000000000000 ) ) ;
#4694 = CARTESIAN_POINT ( 'NONE',  ( -4.171729424061791036, 70.53000000000001535, 12.83926296998457239 ) ) ;
#4695 = DIRECTION ( 'NONE',  ( 0.000000000000000000, -0.000000000000000000, 1.000000000000000000 ) ) ;
#4696 = CARTESIAN_POINT ( 'NONE',  ( 11.57644837279713634, 63.17112552278116056, 6.945208394352803793 ) ) ;
#4697 = CARTESIAN_POINT ( 'NONE',  ( 0.5720401143641312691, 41.70056841707977924, 13.48815436162953496 ) ) ;
#4698 = CARTESIAN_POINT ( 'NONE',  ( 8.474790154542958476, 48.85557007193735046, -10.50863980086850624 ) ) ;
#4699 = CARTESIAN_POINT ( 'NONE',  ( 11.76794919243112680, 20.58000000000001251, -3.823638476888993942 ) ) ;
#4700 = ORIENTED_EDGE ( 'NONE', *, *, #10545, .F. ) ;
#4701 = CARTESIAN_POINT ( 'NONE',  ( 7.272992578804311492, 64.87999999999999545, -10.01041549318726886 ) ) ;
#4702 = CARTESIAN_POINT ( 'NONE',  ( -11.37500000000039790, -35.41562499999989200, 4.711679271993001628 ) ) ;
#4703 = CARTESIAN_POINT ( 'NONE',  ( -4.711679271993003404, -21.85312499999994884, -11.37500000000039435 ) ) ;
#4704 = CARTESIAN_POINT ( 'NONE',  ( -8.549982208541774191E-16, -0.3199999999999986189, 14.19474002721660355 ) ) ;
#4705 = CARTESIAN_POINT ( 'NONE',  ( -0.4211686846404315565, 43.19514363978697702, -13.49345797000271752 ) ) ;
#4706 = CARTESIAN_POINT ( 'NONE',  ( -9.639429313053440751, 80.92999999999996419, -7.743379967852192181 ) ) ;
#4707 = CIRCLE ( 'NONE', #8111, 13.50000000000000000 ) ;
#4708 = CARTESIAN_POINT ( 'NONE',  ( -13.16986379960055231, -60.35624999999985363, 13.16986379959834252 ) ) ;
#4709 = CARTESIAN_POINT ( 'NONE',  ( 5.326996769190816217, 65.87277302910042920, 12.40504085361147801 ) ) ;
#4710 = DIRECTION ( 'NONE',  ( -0.000000000000000000, 1.000000000000000000, -0.000000000000000000 ) ) ;
#4711 = CARTESIAN_POINT ( 'NONE',  ( -7.576616670048093940E-16, 45.67999999999999261, 12.37355403259654985 ) ) ;
#4712 = CARTESIAN_POINT ( 'NONE',  ( 4.171729424061791924, 8.030000000000010019, -12.83926296998457239 ) ) ;
#4713 = CARTESIAN_POINT ( 'NONE',  ( -11.32419978475406097, 46.65450354790017684, -7.349319770073909908 ) ) ;
#4714 = CARTESIAN_POINT ( 'NONE',  ( 12.93101617915861468, 45.56904160174139662, -3.882179959006170744 ) ) ;
#4715 = CARTESIAN_POINT ( 'NONE',  ( 0.1326703767182750571, 70.17522967471386153, -13.49941531153568519 ) ) ;
#4716 = EDGE_CURVE ( 'NONE', #1168, #201, #14556, .T. ) ;
#4717 = CARTESIAN_POINT ( 'NONE',  ( 0.8575635061788081659, 8.007388461842865013, 18.18484536092594439 ) ) ;
#4718 = CARTESIAN_POINT ( 'NONE',  ( 11.82890730580016481, 30.67109828621973477, -6.507028451830479732 ) ) ;
#4719 = CARTESIAN_POINT ( 'NONE',  ( -11.12375258374542852, 56.21798818910362172, 7.649515620900761093 ) ) ;
#4720 = VECTOR ( 'NONE', #759, 1000.000000000000000 ) ;
#4721 = CARTESIAN_POINT ( 'NONE',  ( -1.553272499165753162, 50.62433072722591731, 13.41218807779914357 ) ) ;
#4722 = CARTESIAN_POINT ( 'NONE',  ( 10.75527420406746160, 33.12017030730734746, 8.165193978116038309 ) ) ;
#4723 = CARTESIAN_POINT ( 'NONE',  ( 0.5701897248585299227, 0.02296074491301186918, -12.00000000000000178 ) ) ;
#4724 = CARTESIAN_POINT ( 'NONE',  ( 10.78095112019851243, 39.73819790818856745, -8.130464480974270103 ) ) ;
#4725 = ORIENTED_EDGE ( 'NONE', *, *, #1110, .T. ) ;
#4726 = CARTESIAN_POINT ( 'NONE',  ( -13.47535547316411275, 61.90184251200314947, -0.8153781735254963525 ) ) ;
#4727 = ORIENTED_EDGE ( 'NONE', *, *, #9840, .F. ) ;
#4728 = ORIENTED_EDGE ( 'NONE', *, *, #10160, .F. ) ;
#4729 = CARTESIAN_POINT ( 'NONE',  ( 13.49999999999999822, 30.28000000000000824, 4.386415899144237684 ) ) ;
#4730 = CARTESIAN_POINT ( 'NONE',  ( -18.62499999999935341, -97.78437499999979821, -7.714727599200458030 ) ) ;
#4731 = CARTESIAN_POINT ( 'NONE',  ( 12.90756584819196284, 48.28806130775965499, 3.958932217318702929 ) ) ;
#4732 = CARTESIAN_POINT ( 'NONE',  ( 8.000000000000019540, 0.000000000000000000, -24.73863375370596174 ) ) ;
#4733 = CARTESIAN_POINT ( 'NONE',  ( 9.395478811695362253, 78.81154358623695089, -9.694686115291968775 ) ) ;
#4734 = CARTESIAN_POINT ( 'NONE',  ( 7.272992578804308828, 75.98000000000001819, 10.01041549318726709 ) ) ;
#4735 = CARTESIAN_POINT ( 'NONE',  ( -2.394975141653304274, 46.26611428870612741, -13.28591781961343621 ) ) ;
#4736 = DIRECTION ( 'NONE',  ( 0.000000000000000000, -0.000000000000000000, -1.000000000000000000 ) ) ;
#4737 = CARTESIAN_POINT ( 'NONE',  ( -4.711679271994916540, -4.196874999999971934, 11.37499999999960565 ) ) ;
#4738 = CARTESIAN_POINT ( 'NONE',  ( 3.038735707072813153, 53.78933652538139398, 13.15431546165133447 ) ) ;
#4739 = APPLICATION_CONTEXT ( 'automotive_design' ) ;
#4740 = EDGE_LOOP ( 'NONE', ( #7905, #5628, #11657, #7729 ) ) ;
#4741 = FACE_OUTER_BOUND ( 'NONE', #11113, .T. ) ;
#4742 = ORIENTED_EDGE ( 'NONE', *, *, #8030, .T. ) ;
#4743 = DIRECTION ( 'NONE',  ( 0.000000000000000000, 0.000000000000000000, -1.000000000000000000 ) ) ;
#4744 = CARTESIAN_POINT ( 'NONE',  ( -7.562439852726942746, 34.46358584180068618, -11.18616918020162920 ) ) ;
#4745 = CARTESIAN_POINT ( 'NONE',  ( -4.711679271994915652, -18.69687499999997726, 11.37499999999960210 ) ) ;
#4746 = CARTESIAN_POINT ( 'NONE',  ( 8.833285895147833244, 78.02118567081015499, 10.20927156115941692 ) ) ;
#4747 = CYLINDRICAL_SURFACE ( 'NONE', #14341, 13.50000000000000000 ) ;
#4748 = PLANE ( 'NONE',  #10698 ) ;
#4749 = CARTESIAN_POINT ( 'NONE',  ( -7.499999999999996447, -22.25602869842714071, -9.367496997597605457 ) ) ;
#4750 = CARTESIAN_POINT ( 'NONE',  ( 12.73193533167149383, 72.59359374908758866, -4.534872268809349904 ) ) ;
#4751 = CARTESIAN_POINT ( 'NONE',  ( 3.636496289402157078, 33.03000000000000114, -11.19198476289190936 ) ) ;
#4752 = CARTESIAN_POINT ( 'NONE',  ( 10.92172942406179104, 54.73000000000000398, -7.935100905948385908 ) ) ;
#4753 = CARTESIAN_POINT ( 'NONE',  ( -2.454226844576152811, 52.26824491471117540, -13.27505143425381640 ) ) ;
#4754 = CARTESIAN_POINT ( 'NONE',  ( -11.76794919243112325, -14.22000000000000242, -3.823638476888998827 ) ) ;
#4755 = CARTESIAN_POINT ( 'NONE',  ( -4.171729424061791036, 52.53000000000000114, 12.83926296998457239 ) ) ;
#4756 = EDGE_CURVE ( 'NONE', #9435, #16308, #2934, .T. ) ;
#4757 = DIRECTION ( 'NONE',  ( 0.000000000000000000, 0.000000000000000000, -1.000000000000000000 ) ) ;
#4758 = CARTESIAN_POINT ( 'NONE',  ( 2.279995255611139653E-15, -2.819999999999999840, -12.37355403259654985 ) ) ;
#4759 = CARTESIAN_POINT ( 'NONE',  ( -9.390739836095129078, 68.31192509387784639, 9.701155184843470280 ) ) ;
#4760 = CARTESIAN_POINT ( 'NONE',  ( 13.16986379959834075, -14.56874999999996589, 13.16986379960055231 ) ) ;
#4761 = CARTESIAN_POINT ( 'NONE',  ( 0.000000000000000000, 30.93000000000001393, 0.000000000000000000 ) ) ;
#4762 = AXIS2_PLACEMENT_3D ( 'NONE', #7420, #10077, #4757 ) ;
#4763 = CARTESIAN_POINT ( 'NONE',  ( 1.561832610794586538E-12, -37.46249999999991331, -18.62500000000000000 ) ) ;
#4764 = CARTESIAN_POINT ( 'NONE',  ( 11.00000000000001599, 0.000000000000000000, -15.58845726811988364 ) ) ;
#4765 = CARTESIAN_POINT ( 'NONE',  ( 12.00000000000000533, 102.9300000000000210, 1.714505518806294638E-15 ) ) ;
#4766 = CARTESIAN_POINT ( 'NONE',  ( -5.441113646577473872, 5.918584287042170544, -25.42428528562855305 ) ) ;
#4767 = CARTESIAN_POINT ( 'NONE',  ( 4.171729424061789260, 27.82999999999999474, 12.83926296998457239 ) ) ;
#4768 = ORIENTED_EDGE ( 'NONE', *, *, #11319, .T. ) ;
#4769 = CARTESIAN_POINT ( 'NONE',  ( -7.576616670048093940E-16, 33.67999999999999972, 12.37355403259654807 ) ) ;
#4770 = CARTESIAN_POINT ( 'NONE',  ( 4.171729424061789260, 79.82999999999999829, 12.83926296998457417 ) ) ;
#4771 = CARTESIAN_POINT ( 'NONE',  ( -12.59586300201226905, 32.10615256030042275, 4.857418912420909507 ) ) ;
#4772 = CARTESIAN_POINT ( 'NONE',  ( 0.000000000000000000, -28.00000000000000000, 0.000000000000000000 ) ) ;
#4773 = EDGE_CURVE ( 'NONE', #6360, #1191, #12506, .T. ) ;
#4774 = LINE ( 'NONE', #6113, #11646 ) ;
#4775 = AXIS2_PLACEMENT_3D ( 'NONE', #6762, #9511, #2928 ) ;
#4776 = CARTESIAN_POINT ( 'NONE',  ( 11.76794919243112680, 31.57999999999999119, -3.823638476888993942 ) ) ;
#4777 = CARTESIAN_POINT ( 'NONE',  ( 12.59636570365032604, 51.60610490905947501, -4.856197627295611774 ) ) ;
#4778 = CARTESIAN_POINT ( 'NONE',  ( -12.04821575658347399, 38.15737380506738674, 6.178014121549161075 ) ) ;
#4779 = CARTESIAN_POINT ( 'NONE',  ( 11.44150878627701218, 36.69798984994930180, -7.166082743125198995 ) ) ;
#4780 = CARTESIAN_POINT ( 'NONE',  ( 4.711679271994909435, -86.37187499999978968, -11.37499999999960387 ) ) ;
#4781 = CARTESIAN_POINT ( 'NONE',  ( -2.138189944381240881, 70.60311857767972299, 13.49999999999999822 ) ) ;
#4782 = CARTESIAN_POINT ( 'NONE',  ( 18.99999999999999289, 0.000000000000000000, 1.732050807568941586 ) ) ;
#4783 = CARTESIAN_POINT ( 'NONE',  ( -4.175698386514455684, 80.52985464586872411, 12.83807197239628195 ) ) ;
#4784 = DIRECTION ( 'NONE',  ( -0.000000000000000000, 1.000000000000000000, -0.000000000000000000 ) ) ;
#4785 = CARTESIAN_POINT ( 'NONE',  ( 13.49548971893528915, 48.41801641569664127, 0.3489674621406130828 ) ) ;
#4786 =( GEOMETRIC_REPRESENTATION_CONTEXT ( 3 ) GLOBAL_UNCERTAINTY_ASSIGNED_CONTEXT ( ( #3254 ) ) GLOBAL_UNIT_ASSIGNED_CONTEXT ( ( #14174, #17181, #6420 ) ) REPRESENTATION_CONTEXT ( 'NONE', 'WORKASPACE' ) );
#4787 = CARTESIAN_POINT ( 'NONE',  ( 7.272992578804308828, 16.98000000000000753, 10.01041549318726709 ) ) ;
#4788 = ORIENTED_EDGE ( 'NONE', *, *, #7738, .T. ) ;
#4789 = CARTESIAN_POINT ( 'NONE',  ( 11.76794919243112325, 64.27999999999998693, 3.823638476888997051 ) ) ;
#4790 = CARTESIAN_POINT ( 'NONE',  ( 11.37500000000000178, -26.04999999999992255, 9.531744055041752924E-13 ) ) ;
#4791 = CARTESIAN_POINT ( 'NONE',  ( 4.171729424061791924, 57.02999999999999403, -12.83926296998457239 ) ) ;
#4792 = CARTESIAN_POINT ( 'NONE',  ( -4.171729424061787483, 1.329999999999997851, -12.83926296998457417 ) ) ;
#4793 = CARTESIAN_POINT ( 'NONE',  ( -7.272992578804310604, 31.38000000000002032, 10.01041549318726709 ) ) ;
#4794 = CARTESIAN_POINT ( 'NONE',  ( 2.991272544791215182, 76.07245980423030574, -13.16609516694613013 ) ) ;
#4795 = CARTESIAN_POINT ( 'NONE',  ( -7.714727599197334307, -38.50312499999991189, -18.62500000000064304 ) ) ;
#4796 = CARTESIAN_POINT ( 'NONE',  ( 7.827816212328980505, 65.97516117987781570, 11.00319993222369774 ) ) ;
#4797 = CARTESIAN_POINT ( 'NONE',  ( 13.49999999999999822, 78.28000000000000114, 4.386415899144237684 ) ) ;
#4798 = CARTESIAN_POINT ( 'NONE',  ( 7.272992578804311492, 52.87999999999998835, -10.01041549318726709 ) ) ;
#4799 = CARTESIAN_POINT ( 'NONE',  ( -9.857808185263392531, 59.28819691158693672, 9.223707725319705730 ) ) ;
#4800 = CARTESIAN_POINT ( 'NONE',  ( 13.47549715633743972, 45.40126855624355784, 0.8316350769568319201 ) ) ;
#4801 = CARTESIAN_POINT ( 'NONE',  ( 5.637257242016931791, 69.97526884685950677, -12.26667565995465559 ) ) ;
#4802 = CARTESIAN_POINT ( 'NONE',  ( 6.767892274421971166, 80.93000000000000682, 11.68099457074693603 ) ) ;
#4803 = CARTESIAN_POINT ( 'NONE',  ( 13.46162618359535479, 30.46568736832789526, -1.030778076480221239 ) ) ;
#4804 = CARTESIAN_POINT ( 'NONE',  ( -9.881254368068633553, 56.28734683505406622, 9.209166116772257382 ) ) ;
#4805 = CYLINDRICAL_SURFACE ( 'NONE', #6974, 13.50000000000000000 ) ;
#4806 = CARTESIAN_POINT ( 'NONE',  ( 2.751218558133481817, 64.08107632749974414, -13.21668710184735929 ) ) ;
#4807 = CARTESIAN_POINT ( 'NONE',  ( 0.1477893832224585757, 43.17470362251723515, -13.49930464728724289 ) ) ;
#4808 = CARTESIAN_POINT ( 'NONE',  ( 11.00470575586250810, 39.72507583716802060, -7.820951810514976010 ) ) ;
#4809 = ORIENTED_EDGE ( 'NONE', *, *, #7493, .F. ) ;
#4810 = CARTESIAN_POINT ( 'NONE',  ( -13.48302807339056741, 61.90651663121243331, -0.6789273804275641755 ) ) ;
#4811 = VERTEX_POINT ( 'NONE', #13549 ) ;
#4812 = ORIENTED_EDGE ( 'NONE', *, *, #13733, .T. ) ;
#4813 = CARTESIAN_POINT ( 'NONE',  ( -13.49999999999999822, 29.08000000000000185, 4.386415899144235908 ) ) ;
#4814 = CARTESIAN_POINT ( 'NONE',  ( -7.714727599200467800, -28.09687499999992966, 18.62499999999934630 ) ) ;
#4815 = EDGE_CURVE ( 'NONE', #13318, #16628, #8155, .T. ) ;
#4816 = CARTESIAN_POINT ( 'NONE',  ( 13.06962153774350632, 48.30957997059271491, 3.381577084613068163 ) ) ;
#4817 = CARTESIAN_POINT ( 'NONE',  ( 7.964522300346896344, 57.87871040425520874, -10.90125341165491157 ) ) ;
#4818 = CARTESIAN_POINT ( 'NONE',  ( 1.955722316818022888, 79.10969806729961817, -13.35880382187874282 ) ) ;
#4819 = CARTESIAN_POINT ( 'NONE',  ( -3.636496289402153081, 80.32999999999999829, -11.19198476289190936 ) ) ;
#4820 = CARTESIAN_POINT ( 'NONE',  ( 4.171729424061789260, 40.82999999999999829, 12.83926296998457417 ) ) ;
#4821 = CYLINDRICAL_SURFACE ( 'NONE', #7888, 9.000000000000000000 ) ;
#4822 = CARTESIAN_POINT ( 'NONE',  ( 13.50000000000000355, 41.57999999999999119, -4.386415899144233244 ) ) ;
#4823 = CARTESIAN_POINT ( 'NONE',  ( -4.711679271993003404, -31.25312499999991545, -11.37500000000039613 ) ) ;
#4824 = CARTESIAN_POINT ( 'NONE',  ( -10.92172942406178926, 72.62999999999999545, -7.935100905948389460 ) ) ;
#4825 = CARTESIAN_POINT ( 'NONE',  ( 10.29729702274682701, 33.76497182664475361, -8.730269506234060728 ) ) ;
#4826 = VERTEX_POINT ( 'NONE', #4015 ) ;
#4827 = FACE_BOUND ( 'NONE', #15237, .T. ) ;
#4828 = ORIENTED_EDGE ( 'NONE', *, *, #14194, .F. ) ;
#4829 = CARTESIAN_POINT ( 'NONE',  ( 3.016341264242877962, 67.07153834722653585, -13.15950437981546628 ) ) ;
#4830 = CARTESIAN_POINT ( 'NONE',  ( -11.37499999999999645, -32.22499999999993747, -9.545674412382054647E-13 ) ) ;
#4831 = DIRECTION ( 'NONE',  ( 0.000000000000000000, -1.000000000000000000, 0.000000000000000000 ) ) ;
#4832 = CARTESIAN_POINT ( 'NONE',  ( -5.673995304191476130, 59.47382727098472088, 12.25757816507847942 ) ) ;
#4833 = DIRECTION ( 'NONE',  ( 0.000000000000000000, 1.000000000000000000, 0.000000000000000000 ) ) ;
#4834 = EDGE_CURVE ( 'NONE', #2392, #7733, #9971, .T. ) ;
#4835 = PLANE ( 'NONE',  #2889 ) ;
#4836 = CARTESIAN_POINT ( 'NONE',  ( 11.65143199204702640, 72.68378159801741845, -6.819995948022331334 ) ) ;
#4837 = CARTESIAN_POINT ( 'NONE',  ( 11.76794919243112680, 32.58000000000001251, -3.823638476888993942 ) ) ;
#4838 = CARTESIAN_POINT ( 'NONE',  ( -8.691771469529815392E-16, 53.67999999999999972, 14.19474002721660355 ) ) ;
#4839 = CARTESIAN_POINT ( 'NONE',  ( -3.112744993334869648, 52.29192044083434610, -13.14449540143910511 ) ) ;
#4840 = LINE ( 'NONE', #17024, #14619 ) ;
#4841 = CARTESIAN_POINT ( 'NONE',  ( 1.561832610794586538E-12, -54.11249999999986926, -18.62500000000000000 ) ) ;
#4842 = CARTESIAN_POINT ( 'NONE',  ( -8.605926364152821861, 68.34948858320100840, 10.40136348367510521 ) ) ;
#4843 = CARTESIAN_POINT ( 'NONE',  ( -7.714727599200467800, -61.39687499999984510, 18.62499999999934630 ) ) ;
#4844 = CARTESIAN_POINT ( 'NONE',  ( -8.343458848123582072, 5.379999999999995453, 11.48378591275253768 ) ) ;
#4845 = CARTESIAN_POINT ( 'NONE',  ( -18.62500000000000000, -8.324999999999979750, -1.562973063126292555E-12 ) ) ;
#4846 = CARTESIAN_POINT ( 'NONE',  ( -5.145432190156538077, 65.49406957235127891, 12.48100614422567567 ) ) ;
#4847 = CARTESIAN_POINT ( 'NONE',  ( -24.73863375370587292, 0.000000000000000000, -8.000000000000280664 ) ) ;
#4848 = CARTESIAN_POINT ( 'NONE',  ( 8.000000000000023093, 7.773118517290098062, -17.32050807568876394 ) ) ;
#4849 = CARTESIAN_POINT ( 'NONE',  ( -13.50000000000000000, 23.93000000000000682, -3.469446951953614189E-15 ) ) ;
#4850 = ORIENTED_EDGE ( 'NONE', *, *, #16834, .F. ) ;
#4851 = CARTESIAN_POINT ( 'NONE',  ( 7.272992578804311492, 31.87999999999999190, -10.01041549318726886 ) ) ;
#4852 = CARTESIAN_POINT ( 'NONE',  ( -15.28534784291415249, 6.548267719634618622, 18.06260399879734990 ) ) ;
#4853 = FACE_OUTER_BOUND ( 'NONE', #11810, .T. ) ;
#4854 = EDGE_CURVE ( 'NONE', #1275, #15564, #11760, .T. ) ;
#4855 = CARTESIAN_POINT ( 'NONE',  ( -13.35352338939232908, 31.99944910354191663, 1.983290760110415496 ) ) ;
#4856 = CARTESIAN_POINT ( 'NONE',  ( 1.328818477845309154, 74.72777941065712071, 13.43444295586212966 ) ) ;
#4857 = CARTESIAN_POINT ( 'NONE',  ( 13.00822605418956179, 60.30103388586579882, 3.611571338210629811 ) ) ;
#4858 = CARTESIAN_POINT ( 'NONE',  ( 0.000000000000000000, 80.93000000000000682, -13.50000000000000000 ) ) ;
#4859 = VECTOR ( 'NONE', #16544, 1000.000000000000000 ) ;
#4860 = CARTESIAN_POINT ( 'NONE',  ( 4.171729424061789260, 76.83000000000001251, 12.83926296998457417 ) ) ;
#4861 = CARTESIAN_POINT ( 'NONE',  ( 13.48501078242496654, 51.39964884254468558, 0.8735145204809163788 ) ) ;
#4862 = CARTESIAN_POINT ( 'NONE',  ( -8.224415399157907203, 38.36732905943534888, 10.71480048592647272 ) ) ;
#4863 = CARTESIAN_POINT ( 'NONE',  ( 9.386110757463605125, 36.81227025756452775, -9.712354000322354963 ) ) ;
#4864 = CARTESIAN_POINT ( 'NONE',  ( 11.37499999999960210, -22.85937499999996092, 4.711679271994916540 ) ) ;
#4865 = CARTESIAN_POINT ( 'NONE',  ( -4.023268246324633536E-14, 69.18000000000000682, -13.50000000000000000 ) ) ;
#4866 = CARTESIAN_POINT ( 'NONE',  ( -3.068676428938670764, 77.56962524474758425, 13.14846988648537973 ) ) ;
#4867 = VECTOR ( 'NONE', #8986, 1000.000000000000000 ) ;
#4868 = CARTESIAN_POINT ( 'NONE',  ( -13.49999999999999822, 60.78000000000000114, -4.386415899144240349 ) ) ;
#4869 = CARTESIAN_POINT ( 'NONE',  ( 7.499999999999998224, 88.93000000000000682, 9.367496997597600128 ) ) ;
#4870 = CARTESIAN_POINT ( 'NONE',  ( 10.68025330336615042, 48.74383335475763346, -8.257267871943595239 ) ) ;
#4871 = CARTESIAN_POINT ( 'NONE',  ( -7.272992578804310604, 16.37999999999999901, 10.01041549318726709 ) ) ;
#4872 = VERTEX_POINT ( 'NONE', #14862 ) ;
#4873 = CARTESIAN_POINT ( 'NONE',  ( 9.520470885617715595, 61.13000000000000256, 6.917026985038134512 ) ) ;
#4874 = CARTESIAN_POINT ( 'NONE',  ( 7.714727599197340524, -72.87812499999979821, 18.62500000000063949 ) ) ;
#4875 = CARTESIAN_POINT ( 'NONE',  ( 8.343458848123583849, 56.88000000000000256, -11.48378591275253768 ) ) ;
#4876 = CARTESIAN_POINT ( 'NONE',  ( 8.343458848123583849, -2.120000000000000107, -11.48378591275253768 ) ) ;
#4877 = CARTESIAN_POINT ( 'NONE',  ( 7.272992578804308828, 28.98000000000000398, 10.01041549318726709 ) ) ;
#4878 = LINE ( 'NONE', #3280, #1451 ) ;
#4879 = CARTESIAN_POINT ( 'NONE',  ( 18.62500000000064304, -50.99062499999988063, -7.714727599197334307 ) ) ;
#4880 = FACE_OUTER_BOUND ( 'NONE', #18, .T. ) ;
#4881 = CARTESIAN_POINT ( 'NONE',  ( -9.520470885617717371, 48.23000000000000398, 6.917026985038133624 ) ) ;
#4882 = FACE_BOUND ( 'NONE', #7533, .T. ) ;
#4883 = AXIS2_PLACEMENT_3D ( 'NONE', #16773, #5843, #16600 ) ;
#4884 = CARTESIAN_POINT ( 'NONE',  ( -13.47580627843815293, 58.90211067187865979, -0.8079450873288145374 ) ) ;
#4885 = CARTESIAN_POINT ( 'NONE',  ( 13.49590972726846694, 45.41858991162752091, 0.3323335590089481761 ) ) ;
#4886 = CARTESIAN_POINT ( 'NONE',  ( -18.99999999999998224, 0.000000000000000000, -1.732050807569074369 ) ) ;
#4887 = LINE ( 'NONE', #6572, #5549 ) ;
#4888 = CARTESIAN_POINT ( 'NONE',  ( 13.07359181035909046, 30.54984980636906045, -3.366191560203806610 ) ) ;
#4889 = EDGE_CURVE ( 'NONE', #3120, #2392, #13556, .T. ) ;
#4890 = CARTESIAN_POINT ( 'NONE',  ( -13.42161547619133088, 55.98153511078791666, 1.480727477277027360 ) ) ;
#4891 = CARTESIAN_POINT ( 'NONE',  ( -13.45714999850223670, 49.96723316153270389, 1.074876126443667701 ) ) ;
#4892 = CARTESIAN_POINT ( 'NONE',  ( 18.06260399879750267, 6.548267719634618622, -15.28534784291396420 ) ) ;
#4893 = CARTESIAN_POINT ( 'NONE',  ( 2.889960586727556624, 43.07608798778890247, -13.18705226990277168 ) ) ;
#4894 = CARTESIAN_POINT ( 'NONE',  ( 13.22552129195517523, 39.52604716363583037, -2.718968166365361760 ) ) ;
#4895 = ORIENTED_EDGE ( 'NONE', *, *, #1840, .F. ) ;
#4896 = CARTESIAN_POINT ( 'NONE',  ( 2.445080149700053643E-15, 54.17999999999999972, -13.50000000000000000 ) ) ;
#4897 = CARTESIAN_POINT ( 'NONE',  ( -11.22690699968129202, 61.64836490642452560, -7.497176070716886187 ) ) ;
#4898 =( BOUNDED_CURVE ( )  B_SPLINE_CURVE ( 2, ( #9671, #4442, #13530, #5512, #12394, #4171, #14934, #15196, #2826, #8257, #3096, #12304, #13618 ),
 .UNSPECIFIED., .F., .F. ) 
 B_SPLINE_CURVE_WITH_KNOTS ( ( 3, 2, 2, 2, 2, 2, 3 ),
 ( 0.5416666666666666297, 0.5444444444444443976, 0.5500000000000000444, 0.5555555555555555802, 0.5611111111111111160, 0.5666666666666666519, 0.5694444444444444198 ),
 .UNSPECIFIED. ) 
 CURVE ( )  GEOMETRIC_REPRESENTATION_ITEM ( )  RATIONAL_B_SPLINE_CURVE ( ( 0.9755282581475768211, 0.9755282581475768211, 1.000000000000000000, 0.9510565162951535312, 1.000000000000000000, 0.9510565162951535312, 1.000000000000000000, 0.9510565162951535312, 1.000000000000000000, 0.9510565162951535312, 1.000000000000000000, 0.9755282581475768211, 0.9755282581475768211 ) ) 
 REPRESENTATION_ITEM ( '' )  );
#4899 = ORIENTED_EDGE ( 'NONE', *, *, #12334, .F. ) ;
#4900 = ORIENTED_EDGE ( 'NONE', *, *, #15702, .T. ) ;
#4901 = CARTESIAN_POINT ( 'NONE',  ( 4.171729424061791924, 34.03000000000000114, -12.83926296998457239 ) ) ;
#4902 = CARTESIAN_POINT ( 'NONE',  ( 18.62500000000064659, -91.54062499999980673, -7.714727599197336083 ) ) ;
#4903 = CARTESIAN_POINT ( 'NONE',  ( 13.34781774912188546, 48.35712733598928281, 2.080601422126210576 ) ) ;
#4904 = CARTESIAN_POINT ( 'NONE',  ( 2.420781169875645400, 58.09295764678753926, -13.28118368607770172 ) ) ;
#4905 = CARTESIAN_POINT ( 'NONE',  ( 11.42824258410874982, 78.69914800313584635, -7.198334943051281520 ) ) ;
#4906 = CARTESIAN_POINT ( 'NONE',  ( 7.272992578804308828, 78.97999999999998977, 10.01041549318726709 ) ) ;
#4907 = CARTESIAN_POINT ( 'NONE',  ( 10.92172942406179104, 41.72999999999999687, -7.935100905948385908 ) ) ;
#4908 = CARTESIAN_POINT ( 'NONE',  ( 9.520470885617717371, 82.73000000000000398, -6.917026985038131848 ) ) ;
#4909 = CARTESIAN_POINT ( 'NONE',  ( 1.653273178848926472E-15, 80.93000000000000682, 13.50000000000000000 ) ) ;
#4910 = CARTESIAN_POINT ( 'NONE',  ( 0.000000000000000000, 80.93000000000000682, 0.000000000000000000 ) ) ;
#4911 = EDGE_CURVE ( 'NONE', #16538, #9933, #5971, .T. ) ;
#4912 = LINE ( 'NONE', #15579, #9402 ) ;
#4913 = CARTESIAN_POINT ( 'NONE',  ( 11.37499999999960565, -8.359374999999960920, 4.711679271994918317 ) ) ;
#4914 = CARTESIAN_POINT ( 'NONE',  ( 1.442428843286516438, 35.73186409263165331, 13.42278470930840939 ) ) ;
#4915 = CARTESIAN_POINT ( 'NONE',  ( 4.389406115141700759, 34.02213224516504653, -12.76650137279820107 ) ) ;
#4916 = ORIENTED_EDGE ( 'NONE', *, *, #9795, .F. ) ;
#4917 = DIRECTION ( 'NONE',  ( 0.000000000000000000, 0.000000000000000000, 1.000000000000000000 ) ) ;
#4918 = ORIENTED_EDGE ( 'NONE', *, *, #3850, .T. ) ;
#4919 = CARTESIAN_POINT ( 'NONE',  ( 5.197337872768928335, 66.99201906321724209, -12.45956099938747208 ) ) ;
#4920 = CARTESIAN_POINT ( 'NONE',  ( 9.538709233711902776E-13, -87.41249999999979536, -11.37500000000000000 ) ) ;
#4921 = CARTESIAN_POINT ( 'NONE',  ( 1.774688460779562327, 77.74381030479406718, 13.38330506251782204 ) ) ;
#4922 = CARTESIAN_POINT ( 'NONE',  ( 0.000000000000000000, 80.93000000000000682, 0.000000000000000000 ) ) ;
#4923 = CARTESIAN_POINT ( 'NONE',  ( 15.34492079894891603, 7.924935932049796072, 10.35602470258067953 ) ) ;
#4924 = FACE_BOUND ( 'NONE', #11960, .T. ) ;
#4925 = FACE_OUTER_BOUND ( 'NONE', #5648, .T. ) ;
#4926 = CARTESIAN_POINT ( 'NONE',  ( 4.171729424061789260, 56.82999999999999829, 12.83926296998457417 ) ) ;
#4927 = CARTESIAN_POINT ( 'NONE',  ( -3.201505495297523041, 71.56488954480640530, 13.11491780500991311 ) ) ;
#4928 = CARTESIAN_POINT ( 'NONE',  ( 17.99988701463195184, 8.062211464643718628, 0.1761320247422976937 ) ) ;
#4929 = CARTESIAN_POINT ( 'NONE',  ( 7.714727599197338748, -80.12812499999981242, 18.62500000000063949 ) ) ;
#4930 = CARTESIAN_POINT ( 'NONE',  ( -8.642976562267744356, 68.34776206137323129, 10.37064509888684682 ) ) ;
#4931 = CARTESIAN_POINT ( 'NONE',  ( 7.714727599200458030, -69.72187499999982663, -18.62499999999934985 ) ) ;
#4932 = EDGE_CURVE ( 'NONE', #5443, #4826, #7551, .T. ) ;
#4933 = CARTESIAN_POINT ( 'NONE',  ( 9.287700127114062454, 54.81689961847566650, -9.797388458301975689 ) ) ;
#4934 = CARTESIAN_POINT ( 'NONE',  ( -7.714727599197335195, -55.15312499999986784, -18.62500000000064304 ) ) ;
#4935 = CARTESIAN_POINT ( 'NONE',  ( -5.577144119655765842, 65.47773180331512322, 12.29492813050585731 ) ) ;
#4936 = CARTESIAN_POINT ( 'NONE',  ( 10.00000000000135891, 7.983052681821872554, -15.32050807568352191 ) ) ;
#4937 = CIRCLE ( 'NONE', #12839, 26.00000000000000355 ) ;
#4938 = CARTESIAN_POINT ( 'NONE',  ( -1.812176205795150041, 35.61479768570823978, 13.37810765195845519 ) ) ;
#4939 = ORIENTED_EDGE ( 'NONE', *, *, #1090, .F. ) ;
#4940 = CARTESIAN_POINT ( 'NONE',  ( 9.335235950531815854E-15, 8.180000000000005045, -13.50000000000000178 ) ) ;
#4941 = CARTESIAN_POINT ( 'NONE',  ( 9.241419651377785982, 80.82775795770034222, -10.24784889786167774 ) ) ;
#4942 = CARTESIAN_POINT ( 'NONE',  ( -12.61531847087750258, 32.10420026677966376, 4.806648137471639437 ) ) ;
#4943 = CARTESIAN_POINT ( 'NONE',  ( 8.000000000000023093, 7.773118517290098062, -17.32050807568876394 ) ) ;
#4944 = CARTESIAN_POINT ( 'NONE',  ( 10.68453665737815150, 60.11640859769380540, 8.251753631019978386 ) ) ;
#4945 = CARTESIAN_POINT ( 'NONE',  ( -4.171729424061791036, -2.469999999999999751, 12.83926296998457239 ) ) ;
#4946 = DIRECTION ( 'NONE',  ( 0.000000000000000000, -1.000000000000000000, 0.000000000000000000 ) ) ;
#4947 = CARTESIAN_POINT ( 'NONE',  ( 3.636496289402157078, 56.02999999999999403, -11.19198476289190936 ) ) ;
#4948 = DIRECTION ( 'NONE',  ( 0.000000000000000000, 0.000000000000000000, 1.000000000000000000 ) ) ;
#4949 = CARTESIAN_POINT ( 'NONE',  ( 13.48945982917662789, 51.44836422055956859, -0.5335955830629390828 ) ) ;
#4950 = CARTESIAN_POINT ( 'NONE',  ( -11.05767084123177035, 38.22202780657029564, 7.745299231847412536 ) ) ;
#4951 = EDGE_CURVE ( 'NONE', #15482, #8209, #13161, .T. ) ;
#4952 = CARTESIAN_POINT ( 'NONE',  ( 11.99492941862966333, 36.65855328830576809, -6.194533839644177142 ) ) ;
#4953 = CARTESIAN_POINT ( 'NONE',  ( -4.711679271994915652, -68.64687499999988063, 11.37499999999960210 ) ) ;
#4954 = CARTESIAN_POINT ( 'NONE',  ( -5.233730858707171585, 74.49075943819711654, 12.44419822032766376 ) ) ;
#4955 = CARTESIAN_POINT ( 'NONE',  ( -6.367807814168689795, 77.44634757438805650, 11.90382492994284114 ) ) ;
#4956 = CARTESIAN_POINT ( 'NONE',  ( -3.495764761518072916, 80.55428792539511562, 13.04705504019511864 ) ) ;
#4957 = CARTESIAN_POINT ( 'NONE',  ( 7.500000000000000000, 106.2138518220599650, 8.084116494856623092 ) ) ;
#4958 = ORIENTED_EDGE ( 'NONE', *, *, #14546, .F. ) ;
#4959 = CARTESIAN_POINT ( 'NONE',  ( -3.636496289402156190, 13.53000000000001357, 11.19198476289190758 ) ) ;
#4960 = VERTEX_POINT ( 'NONE', #16727 ) ;
#4961 = CARTESIAN_POINT ( 'NONE',  ( -11.76794919243112325, 57.07999999999999829, 3.823638476888994830 ) ) ;
#4962 = CARTESIAN_POINT ( 'NONE',  ( -11.37500000000039613, -9.365624999999976552, 4.711679271993002516 ) ) ;
#4963 = CARTESIAN_POINT ( 'NONE',  ( -8.043339635997654113, -93.65624999999977263, 8.043339635996302306 ) ) ;
#4964 = CARTESIAN_POINT ( 'NONE',  ( -3.565931047808069021, 80.92999999999999261, -12.36697741789391536 ) ) ;
#4965 = CARTESIAN_POINT ( 'NONE',  ( 13.16986379960055054, -52.03124999999987921, -13.16986379959834430 ) ) ;
#4966 = CARTESIAN_POINT ( 'NONE',  ( -8.691771469529815392E-16, 80.68000000000000682, 14.19474002721660355 ) ) ;
#4967 = AXIS2_PLACEMENT_3D ( 'NONE', #10001, #8674, #16687 ) ;
#4968 = CARTESIAN_POINT ( 'NONE',  ( -7.576616670048093940E-16, 54.67999999999999261, 12.37355403259654985 ) ) ;
#4969 = CARTESIAN_POINT ( 'NONE',  ( 7.999999999999904965, 0.000000000000000000, 17.32050807568881368 ) ) ;
#4970 = CARTESIAN_POINT ( 'NONE',  ( -12.32963178104218294, 59.13122713586460577, 5.502663897909060076 ) ) ;
#4971 = CARTESIAN_POINT ( 'NONE',  ( 13.49933328929112264, 45.42501111118324530, 0.1461406261329739054 ) ) ;
#4972 = CARTESIAN_POINT ( 'NONE',  ( 13.41605565035905201, 69.37766445847722707, 1.503147272406539336 ) ) ;
#4973 = CARTESIAN_POINT ( 'NONE',  ( -2.138189944381219565, 67.60311857767970878, 13.50000000000000355 ) ) ;
#4974 = CARTESIAN_POINT ( 'NONE',  ( 13.28617369785314928, 30.34578285407915033, 2.393266104260259208 ) ) ;
#4975 = CARTESIAN_POINT ( 'NONE',  ( -11.18631900104275978, 55.64585107649359941, -7.557541126061750880 ) ) ;
#4976 = CARTESIAN_POINT ( 'NONE',  ( -13.14190856829288379, 50.04143232289781196, 3.139569975885453168 ) ) ;
#4977 = CARTESIAN_POINT ( 'NONE',  ( 4.745372806345461214, 64.00876641970079106, -12.64604413371457525 ) ) ;
#4978 = CARTESIAN_POINT ( 'NONE',  ( 4.325681857567722943, 43.02444320334033989, -12.78825713985152213 ) ) ;
#4979 = CARTESIAN_POINT ( 'NONE',  ( 13.36748020402493964, 39.36365328056236024, 1.894345376098481415 ) ) ;
#4980 = ORIENTED_EDGE ( 'NONE', *, *, #3133, .T. ) ;
#4981 = CARTESIAN_POINT ( 'NONE',  ( -8.014660668667909604, 70.48352739142377743, -10.86416305456324416 ) ) ;
#4982 = CARTESIAN_POINT ( 'NONE',  ( -10.37380102186887321, 61.59903092850272799, -8.640656467602703117 ) ) ;
#4983 = VECTOR ( 'NONE', #9145, 1000.000000000000000 ) ;
#4984 = CARTESIAN_POINT ( 'NONE',  ( 11.76794919243112680, 2.579999999999996962, -3.823638476888993942 ) ) ;
#4985 = ORIENTED_EDGE ( 'NONE', *, *, #6292, .T. ) ;
#4986 = CARTESIAN_POINT ( 'NONE',  ( -12.95148698083498218, 40.79361840698238240, -3.809996331347294873 ) ) ;
#4987 = ORIENTED_EDGE ( 'NONE', *, *, #6378, .F. ) ;
#4988 = CARTESIAN_POINT ( 'NONE',  ( -10.92172942406179104, 29.23000000000000753, 7.935100905948385908 ) ) ;
#4989 = CARTESIAN_POINT ( 'NONE',  ( -18.62500000000000000, -82.17499999999982663, -1.562973063126292757E-12 ) ) ;
#4990 = CARTESIAN_POINT ( 'NONE',  ( 5.597690550215550509, 47.88292748343059202, 12.29688404133074009 ) ) ;
#4991 = CARTESIAN_POINT ( 'NONE',  ( 4.778181653748105440, 58.00785439407665223, -12.62614106855890483 ) ) ;
#4992 = CARTESIAN_POINT ( 'NONE',  ( 11.93212341947577926, 78.66338650403393729, -6.315679433880966975 ) ) ;
#4993 = ADVANCED_FACE ( 'NONE', ( #10041 ), #16557, .T. ) ;
#4994 = CARTESIAN_POINT ( 'NONE',  ( 11.76794919243112325, 82.27999999999998693, 3.823638476888996607 ) ) ;
#4995 = CARTESIAN_POINT ( 'NONE',  ( -10.92172942406179104, 37.22999999999999687, 7.935100905948387684 ) ) ;
#4996 = CARTESIAN_POINT ( 'NONE',  ( 1.732050807568739970, 7.773118517290100726, 19.00000000000000355 ) ) ;
#4997 = AXIS2_PLACEMENT_3D ( 'NONE', #16789, #11152, #4695 ) ;
#4998 = CARTESIAN_POINT ( 'NONE',  ( 2.138189944381238661, 40.75688142232026934, 13.50000000000000000 ) ) ;
#4999 = CARTESIAN_POINT ( 'NONE',  ( 1.469576158976824144E-15, 9.000000000000000000, 12.00000000000000178 ) ) ;
#5000 = CARTESIAN_POINT ( 'NONE',  ( 9.538709233711902776E-13, -30.21249999999990976, -11.37500000000000178 ) ) ;
#5001 =( BOUNDED_CURVE ( )  B_SPLINE_CURVE ( 2, ( #16280, #5435, #2576, #13375, #213, #12410, #14689, #121, #29, #10737, #5618, #1615, #6675 ),
 .UNSPECIFIED., .F., .F. ) 
 B_SPLINE_CURVE_WITH_KNOTS ( ( 3, 2, 2, 2, 2, 2, 3 ),
 ( 0.7083333333333333703, 0.7111111111111111382, 0.7166666666666666741, 0.7222222222222222099, 0.7277777777777777457, 0.7333333333333332815, 0.7361111111111110494 ),
 .UNSPECIFIED. ) 
 CURVE ( )  GEOMETRIC_REPRESENTATION_ITEM ( )  RATIONAL_B_SPLINE_CURVE ( ( 0.9755282581475768211, 0.9755282581475768211, 1.000000000000000000, 0.9510565162951535312, 1.000000000000000000, 0.9510565162951535312, 1.000000000000000000, 0.9510565162951535312, 1.000000000000000000, 0.9510565162951535312, 1.000000000000000000, 0.9755282581475772652, 0.9755282581475768211 ) ) 
 REPRESENTATION_ITEM ( '' )  );
#5002 = LINE ( 'NONE', #9080, #8956 ) ;
#5003 = CARTESIAN_POINT ( 'NONE',  ( 8.296534642002788118, 33.86373860633018751, -10.64977992570600662 ) ) ;
#5004 = CARTESIAN_POINT ( 'NONE',  ( -13.36016819754640750, 73.86216746102554964, -1.938184205018641082 ) ) ;
#5005 = EDGE_LOOP ( 'NONE', ( #3671, #7208 ) ) ;
#5006 = DIRECTION ( 'NONE',  ( 0.000000000000000000, -1.000000000000000000, 0.000000000000000000 ) ) ;
#5007 = ORIENTED_EDGE ( 'NONE', *, *, #11736, .T. ) ;
#5008 = CARTESIAN_POINT ( 'NONE',  ( -8.043339635996300530, -46.79374999999990337, -8.043339635997652337 ) ) ;
#5009 = CARTESIAN_POINT ( 'NONE',  ( -4.023268246324633536E-14, 69.18000000000000682, -13.50000000000000000 ) ) ;
#5010 = CARTESIAN_POINT ( 'NONE',  ( -3.985033859854695937, 59.53671145982129786, 12.89854622073393031 ) ) ;
#5011 = PLANE ( 'NONE',  #15949 ) ;
#5012 = CARTESIAN_POINT ( 'NONE',  ( -4.171729424061787483, 5.330000000000001847, -12.83926296998457417 ) ) ;
#5013 = CARTESIAN_POINT ( 'NONE',  ( -13.49999999999999822, 49.78000000000000114, -4.386415899144240349 ) ) ;
#5014 = CARTESIAN_POINT ( 'NONE',  ( -7.628114507008727507, 71.39355340672105399, 11.14151516845310219 ) ) ;
#5015 = B_SPLINE_CURVE_WITH_KNOTS ( 'NONE', 3,
 ( #7345, #15268, #4511, #4332 ),
 .UNSPECIFIED., .F., .F.,
 ( 4, 4 ),
 ( 0.008723199174958473981, 0.01636875612029861649 ),
 .UNSPECIFIED. ) ;
#5016 = CARTESIAN_POINT ( 'NONE',  ( -18.62499999999935341, -0.03437499999998146899, -7.714727599200458030 ) ) ;
#5017 = CARTESIAN_POINT ( 'NONE',  ( 0.4448257041681634716, 68.69614250464667293, 13.49999999991288213 ) ) ;
#5018 = CARTESIAN_POINT ( 'NONE',  ( 1.561832610794586538E-12, -70.76249999999983231, -18.62500000000000000 ) ) ;
#5019 = CARTESIAN_POINT ( 'NONE',  ( 6.352825135554033942, 54.94695263489539627, -11.91183081968598501 ) ) ;
#5020 = CARTESIAN_POINT ( 'NONE',  ( -11.76794919243112325, 15.78000000000001535, -3.823638476888998827 ) ) ;
#5021 = CARTESIAN_POINT ( 'NONE',  ( -18.62500000000064659, -26.01562499999994671, 7.714727599197335195 ) ) ;
#5022 = CARTESIAN_POINT ( 'NONE',  ( -10.94367429142997850, 65.22875971052661725, 7.916974700845242907 ) ) ;
#5023 = CARTESIAN_POINT ( 'NONE',  ( -11.80607357642263544, 80.93000000000000682, -0.5610838546640731783 ) ) ;
#5024 = CARTESIAN_POINT ( 'NONE',  ( -1.612532095345881933, 35.62201661823903009, 13.40334904042095943 ) ) ;
#5025 = CARTESIAN_POINT ( 'NONE',  ( -4.171729424061791036, 27.52999999999999758, 12.83926296998457239 ) ) ;
#5026 = EDGE_LOOP ( 'NONE', ( #6083, #2238, #3028, #2476 ) ) ;
#5027 = CARTESIAN_POINT ( 'NONE',  ( -13.50000000000000000, 8.929999999999992610, -3.469446951953614189E-15 ) ) ;
#5028 = DIRECTION ( 'NONE',  ( 0.000000000000000000, -1.000000000000000000, 0.000000000000000000 ) ) ;
#5029 = CARTESIAN_POINT ( 'NONE',  ( -4.296388646608581219, 40.33449593194379190, -12.79811344974312881 ) ) ;
#5030 = CARTESIAN_POINT ( 'NONE',  ( -13.46762570571352846, 31.89769696204961846, -0.9344603740635033517 ) ) ;
#5031 = CARTESIAN_POINT ( 'NONE',  ( 0.000000000000000000, -28.00000000000000000, 0.000000000000000000 ) ) ;
#5032 = CARTESIAN_POINT ( 'NONE',  ( 13.20086187186735671, 60.32965506492238461, 2.836544637259669877 ) ) ;
#5033 = EDGE_CURVE ( 'NONE', #6381, #10449, #2145, .T. ) ;
#5034 = CARTESIAN_POINT ( 'NONE',  ( 10.92172942406178926, -10.86999999999999744, 7.935100905948385908 ) ) ;
#5035 = EDGE_CURVE ( 'NONE', #16561, #13897, #6133, .T. ) ;
#5036 = CARTESIAN_POINT ( 'NONE',  ( -3.877293585379739227, 53.54058681617228643, 12.93122935937666185 ) ) ;
#5037 = CARTESIAN_POINT ( 'NONE',  ( 9.520470885617715595, 55.12999999999999545, 6.917026985038134512 ) ) ;
#5038 = SHAPE_DEFINITION_REPRESENTATION ( #8202, #4322 ) ;
#5039 = CARTESIAN_POINT ( 'NONE',  ( 8.343458848123578520, 73.97999999999998977, 11.48378591275254124 ) ) ;
#5040 = CARTESIAN_POINT ( 'NONE',  ( 13.40136960300497826, 51.37320127860066066, 1.628906160047896012 ) ) ;
#5041 = VECTOR ( 'NONE', #1290, 1000.000000000000000 ) ;
#5042 = CARTESIAN_POINT ( 'NONE',  ( -13.31211181591337578, 38.00888502146048609, 2.245302585987761557 ) ) ;
#5043 = CARTESIAN_POINT ( 'NONE',  ( 11.97434507244688184, 36.66013894208906265, -6.234185302249787064 ) ) ;
#5044 = CARTESIAN_POINT ( 'NONE',  ( 9.538709233711902776E-13, -78.01249999999981810, -11.37499999999999645 ) ) ;
#5045 = CARTESIAN_POINT ( 'NONE',  ( -3.458677200775941429, 74.55563874354560028, 13.04943159450400003 ) ) ;
#5046 = CARTESIAN_POINT ( 'NONE',  ( -6.523521772619733206, 77.44003651811182465, 11.81943641442651760 ) ) ;
#5047 = CARTESIAN_POINT ( 'NONE',  ( -4.023268246324633536E-14, 60.18000000000000682, -13.50000000000000000 ) ) ;
#5048 = CARTESIAN_POINT ( 'NONE',  ( 7.500000000000001776, 103.4461236652718696, -9.346045933502386660 ) ) ;
#5049 = ORIENTED_EDGE ( 'NONE', *, *, #12715, .T. ) ;
#5050 = CARTESIAN_POINT ( 'NONE',  ( -3.636496289402152637, 9.330000000000005400, -11.19198476289190936 ) ) ;
#5051 = VERTEX_POINT ( 'NONE', #4463 ) ;
#5052 = CARTESIAN_POINT ( 'NONE',  ( 9.520470885617715595, 58.13000000000000256, 6.917026985038134512 ) ) ;
#5053 = CARTESIAN_POINT ( 'NONE',  ( -8.043339635996304082, -65.59374999999981526, -8.043339635997652337 ) ) ;
#5054 = CARTESIAN_POINT ( 'NONE',  ( 0.000000000000000000, 9.000000000000000000, -12.00000000000000178 ) ) ;
#5055 = CARTESIAN_POINT ( 'NONE',  ( -10.92172942406179104, 2.230000000000009752, 7.935100905948385908 ) ) ;
#5056 = CARTESIAN_POINT ( 'NONE',  ( 12.10419440643161515, 75.64994209057574892, -5.978384200320835618 ) ) ;
#5057 = CIRCLE ( 'NONE', #9582, 26.00000000000000355 ) ;
#5058 = ADVANCED_FACE ( 'NONE', ( #6146 ), #4805, .T. ) ;
#5059 = LINE ( 'NONE', #3981, #5994 ) ;
#5060 = CARTESIAN_POINT ( 'NONE',  ( 2.684808531364387907, 65.77668069368513670, 13.23259810234951672 ) ) ;
#5061 = CARTESIAN_POINT ( 'NONE',  ( -13.50000000000000000, 67.93000000000000682, -3.306546357697853733E-15 ) ) ;
#5062 = CARTESIAN_POINT ( 'NONE',  ( 11.76794919243112325, 43.28000000000000114, 3.823638476888996607 ) ) ;
#5063 = CARTESIAN_POINT ( 'NONE',  ( 2.785879211291982797E-06, 6.680077384874748780, 13.49999999999942979 ) ) ;
#5064 = CARTESIAN_POINT ( 'NONE',  ( -13.38719676025015204, 58.99337602412490611, 1.818195643690203145 ) ) ;
#5065 = CARTESIAN_POINT ( 'NONE',  ( 9.190356918478798320, 45.03834564354057335, 9.888769335142141514 ) ) ;
#5066 = CARTESIAN_POINT ( 'NONE',  ( 11.11381991456607921, 69.71858770960906782, -7.663787684871768313 ) ) ;
#5067 = CARTESIAN_POINT ( 'NONE',  ( 4.092636507115654965, 80.82714932348959280, 12.86485741472674249 ) ) ;
#5068 = CARTESIAN_POINT ( 'NONE',  ( 13.27325193621214972, 30.51706269903375102, -2.471716390437845412 ) ) ;
#5069 = VECTOR ( 'NONE', #7744, 1000.000000000000000 ) ;
#5070 = CARTESIAN_POINT ( 'NONE',  ( -11.98088293444550523, 55.70025900529297758, -6.222366544694983403 ) ) ;
#5071 = CARTESIAN_POINT ( 'NONE',  ( -13.46016075455064254, 49.96588609214764887, 1.036464527647057432 ) ) ;
#5072 = CARTESIAN_POINT ( 'NONE',  ( 7.792390880217984872, 63.88631323827352304, -11.02401972263586494 ) ) ;
#5073 = CARTESIAN_POINT ( 'NONE',  ( 11.91798314216262256, 42.66442715076532011, -6.341270923659345193 ) ) ;
#5074 = CARTESIAN_POINT ( 'NONE',  ( 12.50959235204128284, 39.24543322991454630, 5.075441208484069655 ) ) ;
#5075 = ORIENTED_EDGE ( 'NONE', *, *, #7977, .F. ) ;
#5076 = CARTESIAN_POINT ( 'NONE',  ( -10.27595300512552612, 70.59341302248357408, -8.758023051731081310 ) ) ;
#5077 = CARTESIAN_POINT ( 'NONE',  ( -9.315893856011628671, 61.54410272838872942, -9.782409614841228063 ) ) ;
#5078 = CARTESIAN_POINT ( 'NONE',  ( -3.636496289402156190, 7.530000000000009130, 11.19198476289190758 ) ) ;
#5079 = ORIENTED_EDGE ( 'NONE', *, *, #13650, .T. ) ;
#5080 = CARTESIAN_POINT ( 'NONE',  ( -7.793068910463410326, 40.47363171592833453, -11.02779009344588346 ) ) ;
#5081 = ORIENTED_EDGE ( 'NONE', *, *, #17355, .F. ) ;
#5082 = CARTESIAN_POINT ( 'NONE',  ( -8.549982208541774191E-16, 23.68000000000000327, 14.19474002721660355 ) ) ;
#5083 = CARTESIAN_POINT ( 'NONE',  ( 18.62500000000000000, -99.89999999999976410, 1.560692158462880521E-12 ) ) ;
#5084 = CARTESIAN_POINT ( 'NONE',  ( 3.176854332491030775, 47.79429613678128419, 13.12122346607776890 ) ) ;
#5085 = EDGE_CURVE ( 'NONE', #10490, #10985, #10951, .T. ) ;
#5086 = CARTESIAN_POINT ( 'NONE',  ( 13.23136294834424653, 57.33332165125162305, 2.733612023197712571 ) ) ;
#5087 = CARTESIAN_POINT ( 'NONE',  ( 12.85467642924241183, 78.57828243993452588, -4.127473429646537184 ) ) ;
#5088 = AXIS2_PLACEMENT_3D ( 'NONE', #14325, #11873, #13102 ) ;
#5089 = CARTESIAN_POINT ( 'NONE',  ( 9.520470885617715595, 82.13000000000000966, 6.917026985038134512 ) ) ;
#5090 = CARTESIAN_POINT ( 'NONE',  ( -3.636496289402155746, 81.53000000000000114, 11.19198476289190936 ) ) ;
#5091 = CYLINDRICAL_SURFACE ( 'NONE', #9309, 13.50000000000000000 ) ;
#5092 = CARTESIAN_POINT ( 'NONE',  ( 10.96735208155292973, -99.99999999999997158, 3.443427092386485366 ) ) ;
#5093 = CARTESIAN_POINT ( 'NONE',  ( 0.000000000000000000, 88.93000000000000682, 0.000000000000000000 ) ) ;
#5094 = CARTESIAN_POINT ( 'NONE',  ( -9.552639591052204498E-13, -88.48749999999975557, 11.37500000000000178 ) ) ;
#5095 = FACE_OUTER_BOUND ( 'NONE', #10831, .T. ) ;
#5096 = CARTESIAN_POINT ( 'NONE',  ( 3.075030622404754777, 34.06943319545086979, -13.14513346880981715 ) ) ;
#5097 = CARTESIAN_POINT ( 'NONE',  ( -3.472868589956898955, 73.30492623780139638, -13.04596869824614025 ) ) ;
#5098 = VERTEX_POINT ( 'NONE', #11239 ) ;
#5099 = ORIENTED_EDGE ( 'NONE', *, *, #5543, .T. ) ;
#5100 = CARTESIAN_POINT ( 'NONE',  ( 2.000520122481862502E-14, 76.67999999999999261, 13.50000000000000000 ) ) ;
#5101 = VERTEX_POINT ( 'NONE', #13778 ) ;
#5102 = CARTESIAN_POINT ( 'NONE',  ( -12.87952649464229005, 41.07582668764707989, 4.061290009118315503 ) ) ;
#5103 = CARTESIAN_POINT ( 'NONE',  ( 8.043339635997652337, -92.58124999999978400, -8.043339635996302306 ) ) ;
#5104 = CARTESIAN_POINT ( 'NONE',  ( -2.167233541823554877, 44.60213075612084310, 13.33398610478137769 ) ) ;
#5105 = FACE_OUTER_BOUND ( 'NONE', #131, .T. ) ;
#5106 = CARTESIAN_POINT ( 'NONE',  ( 11.59055319155406139, 66.68791535026535655, -6.921638745017356875 ) ) ;
#5107 = CARTESIAN_POINT ( 'NONE',  ( -10.92172942406179104, 56.23000000000000398, 7.935100905948387684 ) ) ;
#5108 = CARTESIAN_POINT ( 'NONE',  ( -4.501388629725658674, 71.51804696647752735, 12.72743260569431456 ) ) ;
#5109 = AXIS2_PLACEMENT_3D ( 'NONE', #7520, #10349, #2094 ) ;
#5110 = CARTESIAN_POINT ( 'NONE',  ( 7.714727599200458030, -53.07187499999987068, -18.62499999999934985 ) ) ;
#5111 = CARTESIAN_POINT ( 'NONE',  ( -12.83831444568583002, 68.08011178376837336, 4.174688847921135704 ) ) ;
#5112 = CARTESIAN_POINT ( 'NONE',  ( 7.714727599200456254, -29.17187499999991118, -18.62499999999935341 ) ) ;
#5113 = CARTESIAN_POINT ( 'NONE',  ( 3.292662364912134709, 55.06160801123378690, -13.09230389691793306 ) ) ;
#5114 = CARTESIAN_POINT ( 'NONE',  ( 2.279995255611139653E-15, 18.18000000000001393, -12.37355403259654985 ) ) ;
#5115 = CARTESIAN_POINT ( 'NONE',  ( 7.714727599197338748, -13.52812499999996732, 18.62500000000063949 ) ) ;
#5116 = EDGE_CURVE ( 'NONE', #16836, #10403, #2995, .T. ) ;
#5117 = CARTESIAN_POINT ( 'NONE',  ( -11.50465976997115547, 65.19371892221600717, 7.063487139731847719 ) ) ;
#5118 = CARTESIAN_POINT ( 'NONE',  ( 4.299690572160308814E-08, 62.68000119825558869, 13.49999999999999822 ) ) ;
#5119 = CARTESIAN_POINT ( 'NONE',  ( -11.22894223272487046, 35.21150567205079085, 7.494087460015308011 ) ) ;
#5120 = CARTESIAN_POINT ( 'NONE',  ( 13.50000000000000000, 19.43000000000000327, 1.734723475976807094E-15 ) ) ;
#5121 = ORIENTED_EDGE ( 'NONE', *, *, #2507, .T. ) ;
#5122 = CARTESIAN_POINT ( 'NONE',  ( 0.000000000000000000, 3.000000000000000000, 0.000000000000000000 ) ) ;
#5123 = CARTESIAN_POINT ( 'NONE',  ( -13.47177724509586483, 31.89980168472233402, -0.8729076666594210998 ) ) ;
#5124 = FACE_OUTER_BOUND ( 'NONE', #12172, .T. ) ;
#5125 = CARTESIAN_POINT ( 'NONE',  ( 7.219420632988450492, 59.94908418118669147, 11.40963323477301472 ) ) ;
#5126 = CARTESIAN_POINT ( 'NONE',  ( -8.343458848123582072, -5.620000000000006324, 11.48378591275254124 ) ) ;
#5127 = CARTESIAN_POINT ( 'NONE',  ( -4.436382084028307915, 53.52041252290905504, 12.75888727614251650 ) ) ;
#5128 = CARTESIAN_POINT ( 'NONE',  ( -7.272992578804307939, 59.48000000000000398, -10.01041549318726886 ) ) ;
#5129 = CARTESIAN_POINT ( 'NONE',  ( -13.50000000000000000, 72.92999999999999261, -3.306546357697853733E-15 ) ) ;
#5130 = CARTESIAN_POINT ( 'NONE',  ( 12.48710485657553804, 51.24329990980355376, 5.130518657651855996 ) ) ;
#5131 = CARTESIAN_POINT ( 'NONE',  ( -9.337699186879977020, 38.31443680239338789, 9.749747033323940215 ) ) ;
#5132 = CARTESIAN_POINT ( 'NONE',  ( 11.23610652242876107, 36.71105984972950864, -7.483311881068123839 ) ) ;
#5133 = CARTESIAN_POINT ( 'NONE',  ( -8.043339635996300530, -80.09374999999982947, -8.043339635997652337 ) ) ;
#5134 = ADVANCED_FACE ( 'NONE', ( #7176 ), #450, .F. ) ;
#5135 = DIRECTION ( 'NONE',  ( 1.000000000000000000, 0.000000000000000000, 0.000000000000000000 ) ) ;
#5136 = CARTESIAN_POINT ( 'NONE',  ( -12.16888219137197602, 77.14468546548981465, 5.845481969467562600 ) ) ;
#5137 = CARTESIAN_POINT ( 'NONE',  ( -7.123498274578269118, 79.44487204299775840, -11.46975519674731459 ) ) ;
#5138 = CARTESIAN_POINT ( 'NONE',  ( 7.499999999999998224, 104.9408589258552098, 8.949127168380908159 ) ) ;
#5139 = ORIENTED_EDGE ( 'NONE', *, *, #744, .T. ) ;
#5140 = CARTESIAN_POINT ( 'NONE',  ( 11.76794919243112680, 8.579999999999994742, -3.823638476888993942 ) ) ;
#5141 = ORIENTED_EDGE ( 'NONE', *, *, #8742, .T. ) ;
#5142 = CARTESIAN_POINT ( 'NONE',  ( -7.576616670048093940E-16, 54.67999999999999261, 12.37355403259654807 ) ) ;
#5143 = CARTESIAN_POINT ( 'NONE',  ( 11.37500000000039613, -43.74062499999988773, -4.711679271993004292 ) ) ;
#5144 = CARTESIAN_POINT ( 'NONE',  ( -8.043339635996302306, -89.49374999999979252, -8.043339635997654113 ) ) ;
#5145 = CARTESIAN_POINT ( 'NONE',  ( -8.343458848123582072, -6.619999999999994778, 11.48378591275254124 ) ) ;
#5146 = VECTOR ( 'NONE', #3785, 1000.000000000000000 ) ;
#5147 = CARTESIAN_POINT ( 'NONE',  ( 11.21289274167025773, 75.71237501678724868, -7.524009696738541031 ) ) ;
#5148 = CARTESIAN_POINT ( 'NONE',  ( 10.92172942406178926, 68.12999999999999545, 7.935100905948387684 ) ) ;
#5149 = CARTESIAN_POINT ( 'NONE',  ( 1.574810205816248532, 65.73663956441438927, 13.41017204387538442 ) ) ;
#5150 = CARTESIAN_POINT ( 'NONE',  ( 13.50000000000000000, 72.42999999999999261, 1.653273178848926867E-15 ) ) ;
#5151 = CARTESIAN_POINT ( 'NONE',  ( 11.76794919243112680, 37.57999999999999829, -3.823638476888993942 ) ) ;
#5152 = CARTESIAN_POINT ( 'NONE',  ( -13.25214052457024216, 58.83776751653361714, -2.615125762588000224 ) ) ;
#5153 = CARTESIAN_POINT ( 'NONE',  ( 11.39928639567819424, 45.15932595380822079, 7.232671352425048994 ) ) ;
#5154 = CARTESIAN_POINT ( 'NONE',  ( 11.03746613180151215, 69.72319289778489804, -7.773423729612433775 ) ) ;
#5155 = AXIS2_PLACEMENT_3D ( 'NONE', #12121, #6741, #1505 ) ;
#5156 = CARTESIAN_POINT ( 'NONE',  ( -3.708203932499366751, 6.463974596215563473, -11.41267819554184193 ) ) ;
#5157 = CARTESIAN_POINT ( 'NONE',  ( -3.708203932499369859, 4.663974596215568091, 11.41267819554184193 ) ) ;
#5158 = CARTESIAN_POINT ( 'NONE',  ( -4.835225515329382162, 55.35429197270953239, -12.60603724776291656 ) ) ;
#5159 = ADVANCED_FACE ( 'NONE', ( #16617 ), #15188, .F. ) ;
#5160 = CARTESIAN_POINT ( 'NONE',  ( -6.619156144680720999, 50.43619166903473428, 11.77703965849789292 ) ) ;
#5161 = CARTESIAN_POINT ( 'NONE',  ( 6.310916549568529099, 63.94882138232988211, -11.94029056665552702 ) ) ;
#5162 = CARTESIAN_POINT ( 'NONE',  ( 10.98041672999455365, 42.72652285908267089, -7.855008297392397587 ) ) ;
#5163 = CARTESIAN_POINT ( 'NONE',  ( 9.762871203696802169, 39.06670793169961797, 9.331473753957455486 ) ) ;
#5164 = ORIENTED_EDGE ( 'NONE', *, *, #9821, .F. ) ;
#5165 = CARTESIAN_POINT ( 'NONE',  ( -12.86325130802400096, 70.78271567125864294, -4.099968533946731775 ) ) ;
#5166 = CARTESIAN_POINT ( 'NONE',  ( -5.442442773936573275, 61.37717677536036121, -12.36136841408004372 ) ) ;
#5167 = CARTESIAN_POINT ( 'NONE',  ( 7.272992578804308828, 1.980000000000001315, 10.01041549318726709 ) ) ;
#5168 = VERTEX_POINT ( 'NONE', #622 ) ;
#5169 = ORIENTED_EDGE ( 'NONE', *, *, #14361, .T. ) ;
#5170 = CARTESIAN_POINT ( 'NONE',  ( 8.343458848123578520, 26.98000000000001108, 11.48378591275254124 ) ) ;
#5171 = CARTESIAN_POINT ( 'NONE',  ( -13.16986379960055231, -60.35624999999985363, 13.16986379959834252 ) ) ;
#5172 = CARTESIAN_POINT ( 'NONE',  ( 3.042243549217453769, 61.07061215346910643, -13.15276014662998172 ) ) ;
#5173 = CARTESIAN_POINT ( 'NONE',  ( 12.18771478896523064, 57.64319249440018922, -5.807660356779048350 ) ) ;
#5174 = CARTESIAN_POINT ( 'NONE',  ( 7.272992578804311492, 73.88000000000000966, -10.01041549318726709 ) ) ;
#5175 = CARTESIAN_POINT ( 'NONE',  ( -8.343458848123576743, 36.47999999999998977, -11.48378591275254301 ) ) ;
#5176 = CARTESIAN_POINT ( 'NONE',  ( -9.520470885617717371, 81.22999999999998977, 6.917026985038133624 ) ) ;
#5177 = CARTESIAN_POINT ( 'NONE',  ( 4.171729424061791924, 2.030000000000003801, -12.83926296998457239 ) ) ;
#5178 = CARTESIAN_POINT ( 'NONE',  ( 4.418379050281270537, -99.99999999999997158, 13.00880126231396439 ) ) ;
#5179 = CARTESIAN_POINT ( 'NONE',  ( 0.2312350160357779238, 9.999999999999994671, -13.20992764163158917 ) ) ;
#5180 = CARTESIAN_POINT ( 'NONE',  ( -4.711679271993004292, -5.203124999999986677, -11.37500000000039435 ) ) ;
#5181 = AXIS2_PLACEMENT_3D ( 'NONE', #8064, #6911, #13427 ) ;
#5182 = EDGE_CURVE ( 'NONE', #9540, #11531, #14045, .T. ) ;
#5183 = CARTESIAN_POINT ( 'NONE',  ( -7.499999999999996447, 88.93000000000000682, -12.00000000000000178 ) ) ;
#5184 = CARTESIAN_POINT ( 'NONE',  ( 8.086404608413186423, 33.87324810585550239, -10.81069809738593790 ) ) ;
#5185 = CARTESIAN_POINT ( 'NONE',  ( -3.769655809539932179, 73.31549332748073766, -12.96321091462792552 ) ) ;
#5186 = VERTEX_POINT ( 'NONE', #1677 ) ;
#5187 = VERTEX_POINT ( 'NONE', #12476 ) ;
#5188 = CARTESIAN_POINT ( 'NONE',  ( 3.636496289402157078, 77.03000000000000114, -11.19198476289190936 ) ) ;
#5189 = ORIENTED_EDGE ( 'NONE', *, *, #14625, .F. ) ;
#5190 = CARTESIAN_POINT ( 'NONE',  ( -13.50000000000000000, 16.92999999999999972, -3.469446951953614189E-15 ) ) ;
#5191 = CARTESIAN_POINT ( 'NONE',  ( -12.96917948489248040, 41.06450665792823429, 3.758514619347866237 ) ) ;
#5192 = CARTESIAN_POINT ( 'NONE',  ( -13.16986379959834252, -13.49374999999998792, -13.16986379960055409 ) ) ;
#5193 = CARTESIAN_POINT ( 'NONE',  ( -2.614575715703594483, 44.58605660440404961, 13.25095008111780359 ) ) ;
#5194 = CARTESIAN_POINT ( 'NONE',  ( -7.499999999999994671, -22.51433466932076399, 9.346209313438661681 ) ) ;
#5195 = CARTESIAN_POINT ( 'NONE',  ( 11.58370557121411260, 66.68837149964352307, -6.933095401133553715 ) ) ;
#5196 = CARTESIAN_POINT ( 'NONE',  ( 10.92172942406178926, 48.13000000000000256, 7.935100905948387684 ) ) ;
#5197 = CARTESIAN_POINT ( 'NONE',  ( -5.807920978506090570, 71.46861498452221895, 12.18681003659212259 ) ) ;
#5198 = CARTESIAN_POINT ( 'NONE',  ( -13.16986379959834252, -89.49374999999979252, -13.16986379960055054 ) ) ;
#5199 = CARTESIAN_POINT ( 'NONE',  ( -11.68323218641632977, 68.18151092926409262, 6.764040740981662303 ) ) ;
#5200 = CARTESIAN_POINT ( 'NONE',  ( -1.564113515457998370E-12, -5.237499999999969624, 18.62500000000000000 ) ) ;
#5201 = CARTESIAN_POINT ( 'NONE',  ( 3.933372914426268352, 55.03853806791980929, -12.91984279767183885 ) ) ;
#5202 = CARTESIAN_POINT ( 'NONE',  ( -11.76794919243112325, 19.08000000000001606, 3.823638476888994386 ) ) ;
#5203 = CARTESIAN_POINT ( 'NONE',  ( -22.50000000000000355, -18.00000000000000711, -2.204364238465235822E-15 ) ) ;
#5204 = CARTESIAN_POINT ( 'NONE',  ( -13.36843182285373643, 64.99577036403836416, 1.880491479935817445 ) ) ;
#5205 = CARTESIAN_POINT ( 'NONE',  ( -4.441721580454757401, 35.52022541264950206, 12.74838867243934715 ) ) ;
#5206 = CARTESIAN_POINT ( 'NONE',  ( -8.549982208541774191E-16, 18.68000000000001393, 14.19474002721660355 ) ) ;
#5207 = ORIENTED_EDGE ( 'NONE', *, *, #1788, .T. ) ;
#5208 = CARTESIAN_POINT ( 'NONE',  ( -2.138189944381216012, 8.256881422320265784, -13.50000000000000533 ) ) ;
#5209 = CARTESIAN_POINT ( 'NONE',  ( -3.636496289402156190, 28.53000000000000114, 11.19198476289190758 ) ) ;
#5210 = CARTESIAN_POINT ( 'NONE',  ( -5.068380164899249252, 31.36292906761380195, -12.51566991174745702 ) ) ;
#5211 = CARTESIAN_POINT ( 'NONE',  ( 1.228569358179881110, 73.13583881254791663, -13.44621423555252449 ) ) ;
#5212 = CARTESIAN_POINT ( 'NONE',  ( 13.04260590495897532, 60.30576534669085476, 3.484349753159051932 ) ) ;
#5213 = CARTESIAN_POINT ( 'NONE',  ( -13.49999999999999822, -3.220000000000009077, -4.386415899144240349 ) ) ;
#5214 =( BOUNDED_CURVE ( )  B_SPLINE_CURVE ( 2, ( #8327, #13682, #16427, #11230, #6998, #267, #4331, #13941, #5933, #9739, #15085, #8415, #16516 ),
 .UNSPECIFIED., .F., .F. ) 
 B_SPLINE_CURVE_WITH_KNOTS ( ( 3, 2, 2, 2, 2, 2, 3 ),
 ( 0.5972222222222222099, 0.5999999999999999778, 0.6055555555555555136, 0.6111111111111111605, 0.6166666666666666963, 0.6222222222222222321, 0.6250000000000000000 ),
 .UNSPECIFIED. ) 
 CURVE ( )  GEOMETRIC_REPRESENTATION_ITEM ( )  RATIONAL_B_SPLINE_CURVE ( ( 0.9755282581475768211, 0.9755282581475768211, 1.000000000000000000, 0.9510565162951535312, 1.000000000000000000, 0.9510565162951535312, 1.000000000000000000, 0.9510565162951535312, 1.000000000000000000, 0.9510565162951535312, 1.000000000000000000, 0.9755282581475768211, 0.9755282581475768211 ) ) 
 REPRESENTATION_ITEM ( '' )  );
#5215 = CARTESIAN_POINT ( 'NONE',  ( -9.875734236714132308, 53.28725852313749556, 9.204417485957288037 ) ) ;
#5216 = EDGE_CURVE ( 'NONE', #15567, #3801, #7262, .T. ) ;
#5217 = PRODUCT_CONTEXT ( 'NONE', #556, 'mechanical' ) ;
#5218 = CARTESIAN_POINT ( 'NONE',  ( 9.428902991474831907, 51.04980280169728246, 9.671452565076423369 ) ) ;
#5219 = CARTESIAN_POINT ( 'NONE',  ( -10.40656815491510123, 37.60077104023546468, -8.599786994842322230 ) ) ;
#5220 = CLOSED_SHELL ( 'NONE', ( #8223, #7461, #11223, #13969, #11929, #11977 ) ) ;
#5221 = CARTESIAN_POINT ( 'NONE',  ( 9.351852784421879505, 36.04625061253739915, 9.736770932323047134 ) ) ;
#5222 = CARTESIAN_POINT ( 'NONE',  ( 18.62499999999935341, -39.50937499999993463, 7.714727599200469577 ) ) ;
#5223 = CARTESIAN_POINT ( 'NONE',  ( -3.715995504620742462, 74.54638359986023488, 12.98043278505261178 ) ) ;
#5224 = PRODUCT_DEFINITION_SHAPE ( 'NONE', 'NONE',  #17489 ) ;
#5225 = CARTESIAN_POINT ( 'NONE',  ( -3.825492553879640933, 77.54244891512146864, 12.94665650124274947 ) ) ;
#5226 = CARTESIAN_POINT ( 'NONE',  ( -11.44555968023306214, 80.19798584157584287, 7.171502794116832114 ) ) ;
#5227 = CARTESIAN_POINT ( 'NONE',  ( -11.76794919243112325, 12.78000000000000824, -3.823638476888998827 ) ) ;
#5228 = CARTESIAN_POINT ( 'NONE',  ( 7.500000000000000000, 108.7270211387039325, 1.010069558262741918 ) ) ;
#5229 = LINE ( 'NONE', #15894, #16223 ) ;
#5230 = CARTESIAN_POINT ( 'NONE',  ( 7.272992578804311492, 5.879999999999995453, -10.01041549318726709 ) ) ;
#5231 = CARTESIAN_POINT ( 'NONE',  ( 3.636496289402157078, 53.03000000000000114, -11.19198476289190936 ) ) ;
#5232 = CARTESIAN_POINT ( 'NONE',  ( 11.37500000000000178, -42.69999999999988205, 9.531744055041752924E-13 ) ) ;
#5233 = CARTESIAN_POINT ( 'NONE',  ( -18.62500000000064659, -9.365624999999976552, 7.714727599197335195 ) ) ;
#5234 = CARTESIAN_POINT ( 'NONE',  ( -4.171729424061791036, -9.469999999999998863, 12.83926296998457239 ) ) ;
#5235 = CARTESIAN_POINT ( 'NONE',  ( 12.06631813232368344, 75.65296445888444055, -6.054263178453977545 ) ) ;
#5236 = CARTESIAN_POINT ( 'NONE',  ( 4.171729424061791924, 33.02999999999999403, -12.83926296998457239 ) ) ;
#5237 = CARTESIAN_POINT ( 'NONE',  ( 0.3979337702179393532, 65.69430812332862502, 13.49420666704868843 ) ) ;
#5238 = CARTESIAN_POINT ( 'NONE',  ( 3.636496289402154414, 42.82999999999999829, 11.19198476289190936 ) ) ;
#5239 = CARTESIAN_POINT ( 'NONE',  ( 0.000000000000000000, 5.918584287042170544, 0.000000000000000000 ) ) ;
#5240 = CARTESIAN_POINT ( 'NONE',  ( -10.94460162584092622, 58.63120264642423507, -7.905306038853614048 ) ) ;
#5241 = CARTESIAN_POINT ( 'NONE',  ( 2.918937870619084496, 44.78495419697207325, 13.18066017063958384 ) ) ;
#5242 = CARTESIAN_POINT ( 'NONE',  ( 10.21818166811046780, 69.76923834543529779, -8.822804023081456393 ) ) ;
#5243 = LINE ( 'NONE', #14667, #16251 ) ;
#5244 = CARTESIAN_POINT ( 'NONE',  ( 11.11471058409703083, 30.14144794081360601, 7.663010259766935839 ) ) ;
#5245 = CARTESIAN_POINT ( 'NONE',  ( -0.6196186009307830256, 55.20227918106063925, -13.48581699895939678 ) ) ;
#5246 = CARTESIAN_POINT ( 'NONE',  ( -11.13026847521628504, 50.21760025236010705, 7.640326842646127048 ) ) ;
#5247 = CARTESIAN_POINT ( 'NONE',  ( 12.71605810479952758, 63.26620497749446770, 4.535529403342682286 ) ) ;
#5248 = CARTESIAN_POINT ( 'NONE',  ( 8.421811294184292862, 42.85802858309214258, -10.55187809311721558 ) ) ;
#5249 = CARTESIAN_POINT ( 'NONE',  ( 13.50175417813731471, 39.43989184164867368, -0.2898738848101085619 ) ) ;
#5250 = ORIENTED_EDGE ( 'NONE', *, *, #17010, .F. ) ;
#5251 = CARTESIAN_POINT ( 'NONE',  ( -5.799651830195980295, 70.39105055476129280, -12.19207057802755401 ) ) ;
#5252 = CARTESIAN_POINT ( 'NONE',  ( -7.317172661068146233, 61.45307890462790112, -11.34501891446300448 ) ) ;
#5253 = CARTESIAN_POINT ( 'NONE',  ( -7.409984580736203970E-16, 4.680000000000003268, 12.37355403259654985 ) ) ;
#5254 = EDGE_LOOP ( 'NONE', ( #12307, #9674, #10533, #3406 ) ) ;
#5255 = B_SPLINE_CURVE_WITH_KNOTS ( 'NONE', 3,
 ( #3697, #14462, #6452, #13155, #9110, #2351, #7783, #11836, #9198, #14549, #7866, #17298, #5211, #10601, #9719, #66, #4040, #5471, #16406, #16493, #8125, #10946, #1293, #247, #6797, #6708, #14803, #11119, #15155, #10852, #6977, #12085, #16129, #7062, #1380, #17468, #5381, #10767, #9633, #2963, #9455, #12175, #16219, #2696, #16312, #13492, #13746, #4131, #12444, #9543, #4219, #1646, #6889, #14892, #2786, #8217, #4307, #5738, #9809, #14982, #13578, #4398, #1470, #12261, #8307, #157, #5563, #2875, #13662, #329, #1557, #12353, #5652, #11034, #15065, #8393, #8037, #13405, #4836, #767, #11384, #12617, #16933, #505, #16847, #14010, #10239, #12793, #1985, #4750, #3328, #8655, #4488, #8744, #5825, #7411, #5913, #1815, #16670, #418, #11471, #6091, #1733, #10156, #3053, #14188, #7229, #11557, #15506, #679, #3417, #11292, #16583, #4577, #8831, #8482, #3143, #4664, #14101, #9984, #7146, #13833, #9897, #6175, #12532, #15332, #2073, #11209, #15245, #7498, #13921, #12878, #3235, #8568, #1903, #7320, #12704, #591, #6001, #16756, #10071, #15422, #4003, #14601, #2481, #12135, #24, #8003, #14683, #14273, #10648, #9420, #6845, #16011, #5521, #10817, #11643, #7914, #5344, #13453, #14768, #15593, #3917, #12053, #3501, #13289, #1178, #2659, #12223, #8916, #1339, #5262, #2160, #17350, #9334, #2571, #16179, #6756, #7584, #5427, #115, #12963, #13369, #1258, #6589, #6670, #8175, #17431, #845, #6256, #4091 ),
 .UNSPECIFIED., .F., .F.,
 ( 4, 2, 2, 2, 2, 1, 1, 2, 2, 2, 2, 1, 1, 1, 2, 2, 2, 1, 2, 2, 2, 2, 2, 1, 1, 1, 2, 2, 2, 1, 1, 2, 2, 2, 2, 2, 2, 2, 2, 1, 1, 1, 2, 2, 2, 2, 2, 1, 1, 2, 2, 1, 2, 2, 1, 2, 2, 1, 1, 2, 2, 2, 1, 1, 2, 2, 1, 1, 2, 2, 2, 2, 1, 2, 2, 2, 2, 2, 2, 2, 1, 1, 1, 1, 2, 2, 1, 1, 1, 2, 2, 1, 1, 1, 2, 2, 1, 2, 2, 2, 2, 1, 2, 2, 1, 2, 2, 2, 2, 2, 1, 2, 2, 2, 4 ),
 ( 0.1519801020625093646, 0.1522107000347949768, 0.1523259990209377968, 0.1523404113942056215, 0.1523548237674734740, 0.1523836485140091790, 0.1524412980070805890, 0.1529024939516518133, 0.1538248858407942621, 0.1542860817853654865, 0.1543437312784368964, 0.1544013807715083064, 0.1545166797576510986, 0.1547472777299367386, 0.1552084736745079629, 0.1552661231675793452, 0.1552949479141150502, 0.1553237726606507552, 0.1554390716467935751, 0.1556696696190791873, 0.1561308655636504672, 0.1562461645497932594, 0.1562605769230611119, 0.1562749892963289644, 0.1563038140428646694, 0.1563614635359360794, 0.1565920615082216638, 0.1575144533973640293, 0.1579756493419352259, 0.1580909483280780181, 0.1581485978211494281, 0.1581774225676851331, 0.1582062473142208103, 0.1584368452865064225, 0.1593592371756488157, 0.1598204331202200124, 0.1600510310925056245, 0.1601086805855770068, 0.1601663300786484168, 0.1602816290647912090, 0.1607428250093624056, 0.1609734229816479900, 0.1610887219677907822, 0.1611463714608621922, 0.1612040209539335744, 0.1616652168985047433, 0.1618958148707903277, 0.1620111138569331199, 0.1620687633500045022, 0.1620975880965402072, 0.1621120004698080597, 0.1621264128430759122, 0.1630488047322183331, 0.1639711966213607541, 0.1640288461144321364, 0.1640576708609678414, 0.1640864956075035463, 0.1642017945936463386, 0.1644323925659319507, 0.1648935885105031751, 0.1667383722887880171, 0.1676607641779304658, 0.1678913621502160503, 0.1679490116432874602, 0.1679634240165553127, 0.1679706302031892251, 0.1679778363898231652, 0.1680066611363588702, 0.1681219601225017457, 0.1685831560670731921, 0.1695055479562161127, 0.1697361459285018359, 0.1698514449146447114, 0.1699090944077161214, 0.1699667439007875591, 0.1704279398453590333, 0.1713503317345019539, 0.1718115276790734280, 0.1718691771721448658, 0.1718980019186805708, 0.1719268266652163035, 0.1720421256513591790, 0.1722727236236449300, 0.1727339195682164041, 0.1728492185543592796, 0.1728636309276271321, 0.1728780433008949846, 0.1729068680474307174, 0.1729645175405021273, 0.1731951155127878228, 0.1736563114573592137, 0.1737716104435020614, 0.1738004351900377942, 0.1738148475633056467, 0.1738220537499395590, 0.1738292599365734992, 0.1738869094296449092, 0.1741175074019306046, 0.1750398992910733587, 0.1755010952356447218, 0.1757316932079304173, 0.1757605179544661222, 0.1757749303277339747, 0.1757893427010018272, 0.1758469921940732650, 0.1759622911802161127, 0.1778070749585018984, 0.1796518587367876840, 0.1796806834833233890, 0.1797095082298591218, 0.1797671577229305317, 0.1798824567090734072, 0.1801130546813591304, 0.1805742506259305491, 0.1814966425150734142 ),
 .UNSPECIFIED. ) ;
#5256 = ORIENTED_EDGE ( 'NONE', *, *, #9356, .T. ) ;
#5257 = CARTESIAN_POINT ( 'NONE',  ( 2.621994543952811015E-15, 19.18000000000001037, -14.19474002721660355 ) ) ;
#5258 = CARTESIAN_POINT ( 'NONE',  ( 7.714727599197338748, -96.77812499999976126, 18.62500000000063949 ) ) ;
#5259 = CARTESIAN_POINT ( 'NONE',  ( 4.607920928993483933, 61.01406224977615267, -12.68936818568986169 ) ) ;
#5260 = AXIS2_PLACEMENT_3D ( 'NONE', #5581, #5842, #8410 ) ;
#5261 = CARTESIAN_POINT ( 'NONE',  ( 10.92172942406179104, 10.73000000000000398, -7.935100905948385908 ) ) ;
#5262 = CARTESIAN_POINT ( 'NONE',  ( 7.510597098088380719, 71.96138830267196340, 11.21812259324408600 ) ) ;
#5263 = CARTESIAN_POINT ( 'NONE',  ( 12.38525507082440846, 57.62608040142962551, -5.371732038651033214 ) ) ;
#5264 = CARTESIAN_POINT ( 'NONE',  ( 9.520470885617717371, 70.73000000000000398, -6.917026985038131848 ) ) ;
#5265 = CARTESIAN_POINT ( 'NONE',  ( 7.272992578804311492, 73.88000000000000966, -10.01041549318726709 ) ) ;
#5266 = ADVANCED_FACE ( 'NONE', ( #11417 ), #16528, .F. ) ;
#5267 = CARTESIAN_POINT ( 'NONE',  ( -7.103768928370617353, 47.41597804696614560, 11.47982913313177100 ) ) ;
#5268 = DIRECTION ( 'NONE',  ( 0.000000000000000000, 0.000000000000000000, 1.000000000000000000 ) ) ;
#5269 = CARTESIAN_POINT ( 'NONE',  ( 3.808133373400502286, -99.99999999999998579, 14.89041237177510801 ) ) ;
#5270 = CARTESIAN_POINT ( 'NONE',  ( -10.92172942406179104, 76.23000000000000398, 7.935100905948387684 ) ) ;
#5271 = CARTESIAN_POINT ( 'NONE',  ( 9.538709233711902776E-13, -4.162499999999988987, -11.37500000000000000 ) ) ;
#5272 =( GEOMETRIC_REPRESENTATION_CONTEXT ( 3 ) GLOBAL_UNCERTAINTY_ASSIGNED_CONTEXT ( ( #14034 ) ) GLOBAL_UNIT_ASSIGNED_CONTEXT ( ( #8623, #1953, #16898 ) ) REPRESENTATION_CONTEXT ( 'NONE', 'WORKASPACE' ) );
#5273 = CARTESIAN_POINT ( 'NONE',  ( 0.000000000000000000, 80.93000000000000682, -13.50000000000000000 ) ) ;
#5274 = CARTESIAN_POINT ( 'NONE',  ( 13.41211784917930672, 33.48531139465221429, -1.588086113499469709 ) ) ;
#5275 = CARTESIAN_POINT ( 'NONE',  ( -8.646567327866257813, 73.51228972662816830, -10.37015323812492795 ) ) ;
#5276 = EDGE_LOOP ( 'NONE', ( #15741, #1016, #5537, #4987, #1777 ) ) ;
#5277 = ORIENTED_EDGE ( 'NONE', *, *, #4123, .F. ) ;
#5278 = CARTESIAN_POINT ( 'NONE',  ( -11.76794919243112325, 77.77999999999998693, -3.823638476888998827 ) ) ;
#5279 = ORIENTED_EDGE ( 'NONE', *, *, #11955, .F. ) ;
#5280 = CARTESIAN_POINT ( 'NONE',  ( -13.25459942044035522, 41.02077662930307156, 2.572929991539389949 ) ) ;
#5281 = CARTESIAN_POINT ( 'NONE',  ( 4.711679271993006957, -104.0281249999997755, 11.37500000000039257 ) ) ;
#5282 = CARTESIAN_POINT ( 'NONE',  ( -10.13651174585746517, 44.27358713097766696, 8.916350804182590295 ) ) ;
#5283 = CARTESIAN_POINT ( 'NONE',  ( -7.499999999999994671, -27.44685421792581081, -4.091673783487177474 ) ) ;
#5284 = CIRCLE ( 'NONE', #16556, 3.624999999999999556 ) ;
#5285 = CARTESIAN_POINT ( 'NONE',  ( -4.171729424061791036, 47.52999999999999403, 12.83926296998457239 ) ) ;
#5286 = CARTESIAN_POINT ( 'NONE',  ( -3.154529238787930456, 71.56657476481365165, 13.12627027073374997 ) ) ;
#5287 = ADVANCED_FACE ( 'NONE', ( #16877, #363 ), #8686, .T. ) ;
#5288 = CARTESIAN_POINT ( 'NONE',  ( 1.561832610794586740E-12, -46.86249999999987637, -18.62500000000000000 ) ) ;
#5289 = CARTESIAN_POINT ( 'NONE',  ( -13.41193127300099341, 67.98364253050446848, 1.540011178302385098 ) ) ;
#5290 = CARTESIAN_POINT ( 'NONE',  ( 18.62499999999935341, -8.359374999999960920, 7.714727599200469577 ) ) ;
#5291 = CARTESIAN_POINT ( 'NONE',  ( 10.53126001476443641, 54.75216587731950568, -8.446463747446077974 ) ) ;
#5292 = CARTESIAN_POINT ( 'NONE',  ( 11.76794919243112680, 20.58000000000001251, -3.823638476888993942 ) ) ;
#5293 = CARTESIAN_POINT ( 'NONE',  ( 13.16986379959834075, -81.16874999999980389, 13.16986379960055231 ) ) ;
#5294 = CARTESIAN_POINT ( 'NONE',  ( -13.46180875895859863, 64.89487663202089607, -1.014747862443932114 ) ) ;
#5295 = CARTESIAN_POINT ( 'NONE',  ( -2.260798837967500585, 35.59867054265404107, 13.31089883379040195 ) ) ;
#5296 = CARTESIAN_POINT ( 'NONE',  ( -10.92172942406179104, 21.23000000000000043, 7.935100905948385908 ) ) ;
#5297 = ORIENTED_EDGE ( 'NONE', *, *, #9656, .F. ) ;
#5298 = LINE ( 'NONE', #1211, #11540 ) ;
#5299 = CARTESIAN_POINT ( 'NONE',  ( -10.12002213127730599, 31.58559136480824847, -8.935086232216313817 ) ) ;
#5300 = DIRECTION ( 'NONE',  ( 0.000000000000000000, 0.000000000000000000, 1.000000000000000000 ) ) ;
#5301 = CARTESIAN_POINT ( 'NONE',  ( 3.636496289402157078, -11.96999999999999531, -11.19198476289190936 ) ) ;
#5302 = CARTESIAN_POINT ( 'NONE',  ( 6.398260148579073103, 59.91481284056136758, 11.88785343304075504 ) ) ;
#5303 = CARTESIAN_POINT ( 'NONE',  ( -8.343458848123576743, -3.519999999999999130, -11.48378591275254301 ) ) ;
#5304 = CARTESIAN_POINT ( 'NONE',  ( -11.01659837438729639, 53.22442766106070167, 7.802951671792171418 ) ) ;
#5305 = EDGE_CURVE ( 'NONE', #1193, #860, #10100, .T. ) ;
#5306 = CARTESIAN_POINT ( 'NONE',  ( 11.76794919243112680, 49.57999999999999119, -3.823638476888993942 ) ) ;
#5307 = CARTESIAN_POINT ( 'NONE',  ( -10.92172942406178926, 66.62999999999999545, -7.935100905948389460 ) ) ;
#5308 = CARTESIAN_POINT ( 'NONE',  ( 12.17517545768429876, 51.21400524570869095, 5.885944979336298566 ) ) ;
#5309 = CARTESIAN_POINT ( 'NONE',  ( -8.156909919353799054, 37.48992992535880120, -10.75717574548666988 ) ) ;
#5310 = CARTESIAN_POINT ( 'NONE',  ( 12.55356676875865851, 36.24955043834909674, 4.970527845185399585 ) ) ;
#5311 = CARTESIAN_POINT ( 'NONE',  ( -18.62500000000064659, -16.61562499999998010, 7.714727599197333419 ) ) ;
#5312 = CARTESIAN_POINT ( 'NONE',  ( 12.50000000000000000, 98.93000000000002103, 1.224646799147353059E-15 ) ) ;
#5313 = CARTESIAN_POINT ( 'NONE',  ( -12.79026727553113574, 77.08651115985230717, 4.342467306496795132 ) ) ;
#5314 = CARTESIAN_POINT ( 'NONE',  ( -6.837099079481030017, 79.43283332879646252, -11.64115347217222585 ) ) ;
#5315 = CARTESIAN_POINT ( 'NONE',  ( 4.171729424061791924, 5.030000000000006466, -12.83926296998457239 ) ) ;
#5316 = CARTESIAN_POINT ( 'NONE',  ( -3.636496289402156190, 1.530000000000003579, 11.19198476289190758 ) ) ;
#5317 = CARTESIAN_POINT ( 'NONE',  ( -9.520470885617715595, 50.62999999999999545, -6.917026985038136289 ) ) ;
#5318 = CARTESIAN_POINT ( 'NONE',  ( -11.37499999999960743, -49.98437499999987210, -4.711679271994912099 ) ) ;
#5319 = CARTESIAN_POINT ( 'NONE',  ( 13.16986379960055054, -35.38124999999991616, -13.16986379959834430 ) ) ;
#5320 = CARTESIAN_POINT ( 'NONE',  ( 10.92172942406178926, -5.869999999999993001, 7.935100905948385908 ) ) ;
#5321 = DIRECTION ( 'NONE',  ( 0.4999999999999925060, 0.000000000000000000, 0.8660254037844430375 ) ) ;
#5322 = CARTESIAN_POINT ( 'NONE',  ( 12.23302105539664630, 75.63938679806872756, -5.712831750750090087 ) ) ;
#5323 = CARTESIAN_POINT ( 'NONE',  ( -7.714727599200466912, -94.69687499999976410, 18.62499999999934985 ) ) ;
#5324 = CARTESIAN_POINT ( 'NONE',  ( 8.343458848123583849, 50.87999999999999545, -11.48378591275253768 ) ) ;
#5325 = CARTESIAN_POINT ( 'NONE',  ( -11.76794919243112325, 35.92999999999999972, -2.882316262207890869E-15 ) ) ;
#5326 = CARTESIAN_POINT ( 'NONE',  ( -4.326023945792585756, 41.52443083497766452, 12.78812056084685445 ) ) ;
#5327 = CARTESIAN_POINT ( 'NONE',  ( -11.16450694584518821, 58.64450753011422535, -7.589733078635504171 ) ) ;
#5328 = CARTESIAN_POINT ( 'NONE',  ( 3.163029786985204428, 44.79363501894889055, 13.12593006502653381 ) ) ;
#5329 = DIRECTION ( 'NONE',  ( 0.000000000000000000, 0.000000000000000000, 1.000000000000000000 ) ) ;
#5330 = CARTESIAN_POINT ( 'NONE',  ( -1.900613283889030392, 4.737093173895517317, 12.00000000000175859 ) ) ;
#5331 = CARTESIAN_POINT ( 'NONE',  ( -5.403018934253463357, 55.37564755616709533, -12.37835651047473462 ) ) ;
#5332 = CARTESIAN_POINT ( 'NONE',  ( -13.28966059072577544, 49.84642827815817867, -2.375547661775054831 ) ) ;
#5333 = CARTESIAN_POINT ( 'NONE',  ( 11.89192460612368230, 63.66677491408763245, -6.398269676534774852 ) ) ;
#5334 = CARTESIAN_POINT ( 'NONE',  ( 11.89692274447344822, 42.66601371750947891, -6.380819027429124546 ) ) ;
#5335 = CARTESIAN_POINT ( 'NONE',  ( 11.15118288380620193, 39.14369104754556616, 7.609292751937021038 ) ) ;
#5336 = ORIENTED_EDGE ( 'NONE', *, *, #4495, .F. ) ;
#5337 = CARTESIAN_POINT ( 'NONE',  ( -5.975539096150562557, 70.39796680391430073, -12.10731297254534233 ) ) ;
#5338 = CARTESIAN_POINT ( 'NONE',  ( -1.118605446415761540, 61.22016070313634373, -13.45630796219644232 ) ) ;
#5339 = VERTEX_POINT ( 'NONE', #11501 ) ;
#5340 = ORIENTED_EDGE ( 'NONE', *, *, #3261, .T. ) ;
#5341 = CARTESIAN_POINT ( 'NONE',  ( 8.343458848123583849, 24.88000000000000966, -11.48378591275253768 ) ) ;
#5342 = CARTESIAN_POINT ( 'NONE',  ( -1.564113515457998572E-12, -45.78749999999988773, 18.62500000000000000 ) ) ;
#5343 = CARTESIAN_POINT ( 'NONE',  ( -4.171729424061787483, 11.33000000000000718, -12.83926296998457417 ) ) ;
#5344 = CARTESIAN_POINT ( 'NONE',  ( 9.642912583273176352, 72.06081399527650433, 9.448274979317345057 ) ) ;
#5345 = CARTESIAN_POINT ( 'NONE',  ( 13.41714116088561504, 57.48201277496755068, -1.496883884248394470 ) ) ;
#5346 = CARTESIAN_POINT ( 'NONE',  ( -9.520470885617715595, 65.62999999999999545, -6.917026985038136289 ) ) ;
#5347 = CARTESIAN_POINT ( 'NONE',  ( 9.520470885617717371, 76.73000000000000398, -6.917026985038131848 ) ) ;
#5348 = CARTESIAN_POINT ( 'NONE',  ( -3.750474274136188058, 47.54514764475112543, 12.96859104554123832 ) ) ;
#5349 = AXIS2_PLACEMENT_3D ( 'NONE', #14923, #12034, #11950 ) ;
#5350 = DIRECTION ( 'NONE',  ( 0.000000000000000000, -0.000000000000000000, 1.000000000000000000 ) ) ;
#5351 = CARTESIAN_POINT ( 'NONE',  ( 16.01092576086922747, -100.0000000000000000, 8.948334985424596155 ) ) ;
#5352 = CARTESIAN_POINT ( 'NONE',  ( 0.000000000000000000, -28.00000000000000000, -6.000000000000001776 ) ) ;
#5353 = CARTESIAN_POINT ( 'NONE',  ( -11.37499999999960387, -7.284374999999982059, -4.711679271994910323 ) ) ;
#5354 = CARTESIAN_POINT ( 'NONE',  ( 24.73863375370592976, 0.000000000000000000, 8.000000000000104805 ) ) ;
#5355 = CARTESIAN_POINT ( 'NONE',  ( 12.63363789258784919, 33.60376611986286122, -4.802290623392311275 ) ) ;
#5356 = CARTESIAN_POINT ( 'NONE',  ( -8.104139024512610590, 73.48750659267841456, -10.79785279560148048 ) ) ;
#5357 = ORIENTED_EDGE ( 'NONE', *, *, #10854, .F. ) ;
#5358 = ADVANCED_FACE ( 'NONE', ( #3360, #8776 ), #2018, .F. ) ;
#5359 = EDGE_LOOP ( 'NONE', ( #1253, #4347, #15133, #2217 ) ) ;
#5360 = CARTESIAN_POINT ( 'NONE',  ( -7.576616670048093940E-16, 78.67999999999999261, 12.37355403259654807 ) ) ;
#5361 = ORIENTED_EDGE ( 'NONE', *, *, #12372, .F. ) ;
#5362 = CARTESIAN_POINT ( 'NONE',  ( -9.552639591052204498E-13, -102.9874999999997698, 11.37499999999999645 ) ) ;
#5363 = AXIS2_PLACEMENT_3D ( 'NONE', #6573, #7986, #11953 ) ;
#5364 = CARTESIAN_POINT ( 'NONE',  ( -0.5192945675772188130, 44.66132637824818374, 13.49007153335960929 ) ) ;
#5365 = CARTESIAN_POINT ( 'NONE',  ( -7.499999999999995559, -27.45244706754152375, 4.067225351102819353 ) ) ;
#5366 = CARTESIAN_POINT ( 'NONE',  ( -13.49999999999999822, 46.77999999999998693, -4.386415899144240349 ) ) ;
#5367 = CARTESIAN_POINT ( 'NONE',  ( -13.45458289502007787, 70.96834162828989179, 1.106455849619511156 ) ) ;
#5368 = CARTESIAN_POINT ( 'NONE',  ( 13.16986379960055409, -28.13124999999991260, -13.16986379959834430 ) ) ;
#5369 = CARTESIAN_POINT ( 'NONE',  ( -13.49991414957460734, 67.93186668194280742, 0.05455920092559319451 ) ) ;
#5370 = CARTESIAN_POINT ( 'NONE',  ( 7.714727599200458030, -86.37187499999978968, -18.62499999999934985 ) ) ;
#5371 = CARTESIAN_POINT ( 'NONE',  ( 11.64104852335463569, 54.17556994306837481, 6.836414762659024369 ) ) ;
#5372 = CARTESIAN_POINT ( 'NONE',  ( -7.272992578804310604, 16.37999999999999901, 10.01041549318726709 ) ) ;
#5373 = CARTESIAN_POINT ( 'NONE',  ( -1.564113515457998572E-12, -79.08749999999980673, 18.62500000000000000 ) ) ;
#5374 = CARTESIAN_POINT ( 'NONE',  ( -12.96223390259766184, 64.79501674517034360, -3.772551170016495981 ) ) ;
#5375 = EDGE_CURVE ( 'NONE', #2917, #3478, #14924, .T. ) ;
#5376 = VECTOR ( 'NONE', #10089, 1000.000000000000000 ) ;
#5377 = CARTESIAN_POINT ( 'NONE',  ( -13.07700142429071200, 34.81050193234469958, -3.356985455952382402 ) ) ;
#5378 = ORIENTED_EDGE ( 'NONE', *, *, #13862, .T. ) ;
#5379 = CARTESIAN_POINT ( 'NONE',  ( 21.14483242576215716, 7.170662809914417402, -2.970370385949218317 ) ) ;
#5380 = CARTESIAN_POINT ( 'NONE',  ( -1.999421349371006906, 31.25185859380078668, -13.35861204086333309 ) ) ;
#5381 = CARTESIAN_POINT ( 'NONE',  ( 5.857397934039831000, 72.96667994176048921, -12.16334209717476433 ) ) ;
#5382 = CARTESIAN_POINT ( 'NONE',  ( 9.520470885617717371, -9.269999999999999574, -6.917026985038131848 ) ) ;
#5383 = CARTESIAN_POINT ( 'NONE',  ( 4.844150578424402553, 59.85459317586593642, 12.60107945964768561 ) ) ;
#5384 = CARTESIAN_POINT ( 'NONE',  ( 13.49999999999999822, -4.719999999999997975, 4.386415899144237684 ) ) ;
#5385 = CARTESIAN_POINT ( 'NONE',  ( -10.15663687072385635, 53.27256531316408683, 8.895185726361642509 ) ) ;
#5386 = CARTESIAN_POINT ( 'NONE',  ( -7.272992578804310604, 48.38000000000000256, 10.01041549318726709 ) ) ;
#5387 = SHAPE_DEFINITION_REPRESENTATION ( #4235, #7275 ) ;
#5388 = CARTESIAN_POINT ( 'NONE',  ( 13.50000000000000000, 65.43000000000000682, 1.653273178848926867E-15 ) ) ;
#5389 = CARTESIAN_POINT ( 'NONE',  ( 7.529356974007705539, 50.96216477632258091, 11.20855974609861683 ) ) ;
#5390 = CARTESIAN_POINT ( 'NONE',  ( -8.055337278822385372, 37.48536512197566850, -10.83337006914397449 ) ) ;
#5391 =( GEOMETRIC_REPRESENTATION_CONTEXT ( 3 ) GLOBAL_UNCERTAINTY_ASSIGNED_CONTEXT ( ( #1836 ) ) GLOBAL_UNIT_ASSIGNED_CONTEXT ( ( #4602, #3262, #14039 ) ) REPRESENTATION_CONTEXT ( 'NONE', 'WORKASPACE' ) );
#5392 = CARTESIAN_POINT ( 'NONE',  ( 7.123395036261381819, 35.94488704657532452, 11.46981905184369133 ) ) ;
#5393 = CARTESIAN_POINT ( 'NONE',  ( -7.714727599200466912, -35.34687499999993321, 18.62499999999935341 ) ) ;
#5394 = CARTESIAN_POINT ( 'NONE',  ( -11.99030647170363828, 74.15890988944590845, 6.203430717540079797 ) ) ;
#5395 = CARTESIAN_POINT ( 'NONE',  ( -10.92538970018559752, 76.63004364216227771, -7.932434916078520359 ) ) ;
#5396 = EDGE_CURVE ( 'NONE', #5891, #2674, #8583, .T. ) ;
#5397 = CARTESIAN_POINT ( 'NONE',  ( -12.63983531847754627, 79.75770905865978477, -4.762627132487758708 ) ) ;
#5398 = CARTESIAN_POINT ( 'NONE',  ( -7.272992578804307939, 12.48000000000000576, -10.01041549318726886 ) ) ;
#5399 = CARTESIAN_POINT ( 'NONE',  ( -1.218708134006305066, 80.93000000000000682, 12.93996086231513409 ) ) ;
#5400 = CARTESIAN_POINT ( 'NONE',  ( 11.76794919243112325, -0.5699999999999871836, 1.734723475976807094E-15 ) ) ;
#5401 = CARTESIAN_POINT ( 'NONE',  ( -7.272992578804307939, 44.47999999999999687, -10.01041549318727064 ) ) ;
#5402 = CARTESIAN_POINT ( 'NONE',  ( -11.37499999999960387, -40.58437499999990905, -4.711679271994910323 ) ) ;
#5403 = CARTESIAN_POINT ( 'NONE',  ( 1.561832610794586538E-12, -20.81249999999995026, -18.62500000000000000 ) ) ;
#5404 = CARTESIAN_POINT ( 'NONE',  ( -10.92172942406179104, -3.769999999999995577, 7.935100905948385908 ) ) ;
#5405 = CARTESIAN_POINT ( 'NONE',  ( -12.92793998791257337, 40.79065489648220222, -3.889074535841753999 ) ) ;
#5406 = DIRECTION ( 'NONE',  ( -1.000000000000000000, 0.000000000000000000, -1.075706766891313812E-14 ) ) ;
#5407 = CARTESIAN_POINT ( 'NONE',  ( 12.31660755751379632, 75.22787210861035589, 5.528443808838319207 ) ) ;
#5408 = CARTESIAN_POINT ( 'NONE',  ( -7.272992578804310604, 39.38000000000000256, 10.01041549318726709 ) ) ;
#5409 = CARTESIAN_POINT ( 'NONE',  ( -7.190695991324615122, 41.41232216974482583, 11.42629593928715792 ) ) ;
#5410 = CARTESIAN_POINT ( 'NONE',  ( -10.01477406080996424, 58.57944998338118126, -9.064625782096852546 ) ) ;
#5411 = CARTESIAN_POINT ( 'NONE',  ( 4.266835968733136752, 44.83337071590181466, 12.80827659740992175 ) ) ;
#5412 = CARTESIAN_POINT ( 'NONE',  ( 8.343458848123583849, 59.87999999999999545, -11.48378591275253768 ) ) ;
#5413 = DIRECTION ( 'NONE',  ( 0.000000000000000000, -1.000000000000000000, 0.000000000000000000 ) ) ;
#5414 = CARTESIAN_POINT ( 'NONE',  ( -1.900613283907767848, 0.3908560185363838535, -11.99999999999569766 ) ) ;
#5415 = CARTESIAN_POINT ( 'NONE',  ( -7.484330937750101498, 49.46025488201969722, -11.23552342734818055 ) ) ;
#5416 = CARTESIAN_POINT ( 'NONE',  ( 13.42206755560985698, 63.48053927388662743, -1.452603711471143866 ) ) ;
#5417 = CARTESIAN_POINT ( 'NONE',  ( 12.89381267789188534, 42.57361400711115351, -4.003013936710616782 ) ) ;
#5418 = CARTESIAN_POINT ( 'NONE',  ( 1.923701266133974741, 38.74915784931967977, 13.36274881015140359 ) ) ;
#5419 = ORIENTED_EDGE ( 'NONE', *, *, #7512, .F. ) ;
#5420 = DIRECTION ( 'NONE',  ( 0.000000000000000000, 0.000000000000000000, -1.000000000000000000 ) ) ;
#5421 = CARTESIAN_POINT ( 'NONE',  ( 11.37500000000000000, -9.629649721936179265E-32, 9.531744055041752924E-13 ) ) ;
#5422 = ORIENTED_EDGE ( 'NONE', *, *, #3035, .F. ) ;
#5423 = CARTESIAN_POINT ( 'NONE',  ( -5.667801726729744694, 43.38591874923557867, -12.25259268504242804 ) ) ;
#5424 = CARTESIAN_POINT ( 'NONE',  ( 18.62500000000064304, -84.29062499999983515, -7.714727599197335195 ) ) ;
#5425 = CARTESIAN_POINT ( 'NONE',  ( 9.320893742113016245, 60.81526611863908727, -9.765814572247236924 ) ) ;
#5426 = CARTESIAN_POINT ( 'NONE',  ( 4.171729424061791924, 11.03000000000001180, -12.83926296998457239 ) ) ;
#5427 = CARTESIAN_POINT ( 'NONE',  ( 2.452834738616162191, 71.76819877488479449, 13.27530762632762773 ) ) ;
#5428 = CARTESIAN_POINT ( 'NONE',  ( 13.36384259635446803, 57.49692427815710971, -1.912564800906976448 ) ) ;
#5429 = CARTESIAN_POINT ( 'NONE',  ( 3.636496289402154414, 72.83000000000001251, 11.19198476289190936 ) ) ;
#5430 = CARTESIAN_POINT ( 'NONE',  ( -9.520470885617717371, 78.23000000000000398, 6.917026985038133624 ) ) ;
#5431 = VECTOR ( 'NONE', #5697, 1000.000000000000000 ) ;
#5432 = CARTESIAN_POINT ( 'NONE',  ( -7.565627924516670433, 47.39628028002687188, 11.18235063458430467 ) ) ;
#5433 = B_SPLINE_CURVE_WITH_KNOTS ( 'NONE', 3,
 ( #3583, #842, #15675, #12875, #6253, #15502, #8913, #8996, #14443, #14270, #11468, #17103, #764, #16929, #14354, #13049, #3414, #8827, #6172, #2242, #5010, #931, #11554, #4832, #10236, #17018, #15591, #3498, #2157, #11639, #10410, #7670, #6341, #11727, #15767, #3676, #9090, #2330, #16844, #3682, #16981, #4799, #6394, #1069, #6139, #2038, #12843, #7545, #7811, #9142, #10373, #2376, #14318, #14148, #10286, #15905, #14489, #2206, #11776, #10201, #7632, #981, #6482, #13010, #7719, #14234, #8791, #891, #4970, #7462, #731, #13184, #6304, #11518, #15638, #16895, #11867, #11689, #17153, #15553, #17066, #5064, #17242, #15727, #13095, #2119, #3465, #3635, #9049, #8879, #12923, #14401, #807, #6219, #11605, #10459, #3548, #4884, #8962, #10544, #15819, #2290, #3723, #5152, #3895, #5, #1158, #14749, #17328, #13350, #9400, #13606, #2638, #14581, #2462, #9572, #10625, #3814, #15991, #9313, #6568, #13519, #5327, #14663, #4071, #5240, #2552, #11949, #5502, #5410, #7981, #9486, #10711, #16077, #1239, #8069, #12293, #7893, #10797, #6651, #13270, #12033, #1410, #6825, #17412, #1501, #188, #8245, #4159, #6737, #2726, #3984, #10884, #13433, #2816, #1321, #12116, #14832, #16161, #8154, #6915, #12203, #96, #16254, #14922, #5594, #10974, #9227, #14041, #1928, #7351, #11235, #13687, #13859, #11061, #15272, #16612, #9838, #3170, #15010, #12381, #7258 ),
 .UNSPECIFIED., .F., .F.,
 ( 4, 1, 2, 2, 1, 1, 2, 2, 2, 2, 1, 2, 2, 2, 2, 2, 1, 2, 2, 1, 1, 1, 2, 2, 2, 2, 1, 1, 2, 2, 2, 2, 2, 1, 1, 2, 2, 1, 2, 2, 2, 2, 2, 1, 1, 2, 2, 2, 2, 1, 2, 2, 1, 1, 1, 2, 1, 2, 2, 1, 1, 2, 2, 2, 2, 2, 2, 1, 2, 2, 2, 2, 2, 1, 1, 1, 2, 2, 2, 2, 2, 2, 1, 1, 1, 1, 2, 2, 2, 2, 1, 1, 1, 2, 2, 1, 1, 2, 2, 2, 2, 2, 1, 1, 2, 2, 1, 2, 2, 4 ),
 ( 0.4167745338196714999, 0.4168890612373624127, 0.4169176930917851687, 0.4169320090189965189, 0.4169463249462078691, 0.4170035886550533255, 0.4172326434904351511, 0.4176907531611988578, 0.4186069725027261601, 0.4190650821734898668, 0.4192941370088716924, 0.4194086644265626052, 0.4195231918442535179, 0.4204394111857808758, 0.4213556305273082336, 0.4218137401980718848, 0.4219282676157627976, 0.4219354255793684727, 0.4219425835429741478, 0.4219568994701855535, 0.4219855313246083095, 0.4220427950334537659, 0.4222718498688357025, 0.4231880692103633934, 0.4241042885518910843, 0.4243333433872730209, 0.4243906070961184773, 0.4244192389505412333, 0.4244335548777526390, 0.4244478708049639892, 0.4245623982226550130, 0.4250205078934190528, 0.4254786175641831480, 0.4255931449818741719, 0.4256504086907196838, 0.4256790405451423842, 0.4256933564723537899, 0.4257076723995651957, 0.4259367272349471878, 0.4268529465764753228, 0.4273110562472394180, 0.4277691659180034578, 0.4286853852595315928, 0.4291434949302956881, 0.4293725497656777357, 0.4294298134745232476, 0.4294870771833687595, 0.4296016046010597278, 0.4305178239425879183, 0.4306323513602789421, 0.4306896150691243985, 0.4307182469235471545, 0.4307468787779699104, 0.4309759336133519581, 0.4314340432841160533, 0.4318921529548800931, 0.4319207848093028490, 0.4319351007365142547, 0.4319494166637256050, 0.4320066803725711169, 0.4321212077902621407, 0.4323502626256441883, 0.4332664819671723788, 0.4341827013087005138, 0.4344117561440825614, 0.4344403879985053174, 0.4344690198529280734, 0.4345262835617735853, 0.4346408109794646091, 0.4350989206502287043, 0.4369313593332849743, 0.4369456752604963801, 0.4369599911877077303, 0.4369886230421305418, 0.4370458867509760537, 0.4371604141686670775, 0.4373894690040492361, 0.4378475786748134424, 0.4387637980163419105, 0.4392219076871061167, 0.4394509625224882199, 0.4394581204860938950, 0.4394652784496996256, 0.4394795943769110314, 0.4395082262313337873, 0.4395654899401793547, 0.4396800173578704340, 0.4405962366993994017, 0.4415124560409283139, 0.4417415108763105280, 0.4418560382940016074, 0.4419133020028471748, 0.4419419338572699862, 0.4419490918208756614, 0.4419562497844813365, 0.4419705657116927422, 0.4424286753824571705, 0.4428867850532216544, 0.4431158398886038685, 0.4432303673062950033, 0.4433448947239861382, 0.4442611140655150503, 0.4443756414832061297, 0.4444329051920516971, 0.4444472211192631028, 0.4444615370464744530, 0.4444901689008972645, 0.4447192237362794787, 0.4451773334070439625, 0.4460935527485729302 ),
 .UNSPECIFIED. ) ;
#5434 = EDGE_CURVE ( 'NONE', #14697, #10231, #7256, .T. ) ;
#5435 = CARTESIAN_POINT ( 'NONE',  ( -2.138189944381240881, 46.60311857767973009, 13.49999999999999822 ) ) ;
#5436 = CARTESIAN_POINT ( 'NONE',  ( 8.343458848123580296, 73.97999999999998977, 11.48378591275253768 ) ) ;
#5437 = CARTESIAN_POINT ( 'NONE',  ( 10.92172942406179104, 38.73000000000000398, -7.935100905948385908 ) ) ;
#5438 = CARTESIAN_POINT ( 'NONE',  ( -4.171729424061791036, 34.53000000000000114, 12.83926296998457239 ) ) ;
#5439 = CARTESIAN_POINT ( 'NONE',  ( -11.37500000000039790, -85.36562499999978115, 4.711679271993001628 ) ) ;
#5440 = CARTESIAN_POINT ( 'NONE',  ( -8.343458848123582072, 40.37999999999999545, 11.48378591275253768 ) ) ;
#5441 = CARTESIAN_POINT ( 'NONE',  ( 13.44669328521645113, 33.38616000105633219, 1.256905049340288683 ) ) ;
#5442 = CARTESIAN_POINT ( 'NONE',  ( -10.21952983404348458, 73.59082116183350308, -8.824648151853521583 ) ) ;
#5443 = VERTEX_POINT ( 'NONE', #12719 ) ;
#5444 = ORIENTED_EDGE ( 'NONE', *, *, #10059, .T. ) ;
#5445 = CARTESIAN_POINT ( 'NONE',  ( -9.520470885617715595, 24.63000000000001322, -6.917026985038136289 ) ) ;
#5446 = CARTESIAN_POINT ( 'NONE',  ( -2.192110700418634206, 62.60117977606283546, 13.32083775572103512 ) ) ;
#5447 = ORIENTED_EDGE ( 'NONE', *, *, #14402, .T. ) ;
#5448 = VECTOR ( 'NONE', #13295, 1000.000000000000000 ) ;
#5449 = CARTESIAN_POINT ( 'NONE',  ( -13.50304319313545065, 40.92847950508530630, -0.04090659003252928444 ) ) ;
#5450 = CARTESIAN_POINT ( 'NONE',  ( 4.711679271994911211, -93.62187499999978968, -11.37499999999960210 ) ) ;
#5451 = CARTESIAN_POINT ( 'NONE',  ( -11.16075802225499025, 44.21572617453895759, 7.595305378214631808 ) ) ;
#5452 = DIRECTION ( 'NONE',  ( 0.000000000000000000, 0.000000000000000000, -1.000000000000000000 ) ) ;
#5453 = CARTESIAN_POINT ( 'NONE',  ( -4.171729424061787483, 43.32999999999999829, -12.83926296998457417 ) ) ;
#5454 = CARTESIAN_POINT ( 'NONE',  ( -12.93008338321562256, 71.06905249602031915, 3.881103319701416421 ) ) ;
#5455 = EDGE_CURVE ( 'NONE', #14868, #9538, #15125, .T. ) ;
#5456 = AXIS2_PLACEMENT_3D ( 'NONE', #710, #8863, #11500 ) ;
#5457 = CARTESIAN_POINT ( 'NONE',  ( -13.16986379960055409, -53.10624999999986073, 13.16986379959834252 ) ) ;
#5458 = CARTESIAN_POINT ( 'NONE',  ( -12.51906270480975714, 68.11402849159634343, 5.063022440180297679 ) ) ;
#5459 = CARTESIAN_POINT ( 'NONE',  ( 1.561832610794586740E-12, -13.56249999999995026, -18.62500000000000000 ) ) ;
#5460 = CARTESIAN_POINT ( 'NONE',  ( 13.05816527381254666, 54.30794901924826235, 3.425548258310757710 ) ) ;
#5461 = DIRECTION ( 'NONE',  ( 0.000000000000000000, 0.000000000000000000, -1.000000000000000000 ) ) ;
#5462 = CARTESIAN_POINT ( 'NONE',  ( -13.37946240819375632, 64.99289358431782659, 1.800012917707035420 ) ) ;
#5463 = ORIENTED_EDGE ( 'NONE', *, *, #8679, .T. ) ;
#5464 = DIRECTION ( 'NONE',  ( 0.8660254037844399289, 0.000000000000000000, -0.4999999999999977240 ) ) ;
#5465 = CARTESIAN_POINT ( 'NONE',  ( -13.34870812582085264, 35.00060202485487793, 2.015441165875480944 ) ) ;
#5466 = VERTEX_POINT ( 'NONE', #3345 ) ;
#5467 = CARTESIAN_POINT ( 'NONE',  ( -13.16837719205942570, 1.171226224988977633E-15, -1.863363871322652354 ) ) ;
#5468 = SHAPE_REPRESENTATION ( 'Base', ( #16654 ), #13005 ) ;
#5469 = FACE_OUTER_BOUND ( 'NONE', #17121, .T. ) ;
#5470 = CARTESIAN_POINT ( 'NONE',  ( -5.976125424403057274, 31.39799419942340819, -12.10679337452015503 ) ) ;
#5471 = CARTESIAN_POINT ( 'NONE',  ( 3.326001417435852758, 73.06040922954841221, -13.08388940738754158 ) ) ;
#5472 = CARTESIAN_POINT ( 'NONE',  ( -7.409984580736203970E-16, -10.32000000000000384, 12.37355403259654985 ) ) ;
#5473 = DIRECTION ( 'NONE',  ( -0.000000000000000000, -1.000000000000000000, -0.000000000000000000 ) ) ;
#5474 = CARTESIAN_POINT ( 'NONE',  ( 8.343458848123583849, -16.12000000000000810, -11.48378591275253768 ) ) ;
#5475 = CARTESIAN_POINT ( 'NONE',  ( -10.92172942406179104, 74.23000000000000398, 7.935100905948387684 ) ) ;
#5476 = CARTESIAN_POINT ( 'NONE',  ( -13.47854047285069790, 52.90374775157414433, -0.7608956181714418010 ) ) ;
#5477 = CARTESIAN_POINT ( 'NONE',  ( 7.272992578804308828, 51.97999999999998977, 10.01041549318726709 ) ) ;
#5478 = EDGE_CURVE ( 'NONE', #16817, #12239, #8759, .T. ) ;
#5479 = CARTESIAN_POINT ( 'NONE',  ( 3.182817155287316346, 50.79451344581282513, 13.11991552520243154 ) ) ;
#5480 = CARTESIAN_POINT ( 'NONE',  ( -5.657249770757468710, 37.38550904903456029, -12.25752513883166017 ) ) ;
#5481 = CARTESIAN_POINT ( 'NONE',  ( 13.26418904884840977, 36.34139017399488836, 2.514688632223297748 ) ) ;
#5482 = CARTESIAN_POINT ( 'NONE',  ( 7.714727599197340524, -20.77812499999997087, 18.62500000000063949 ) ) ;
#5483 = CARTESIAN_POINT ( 'NONE',  ( -11.97893996698503116, 74.15978608494305035, 6.225358771720943984 ) ) ;
#5484 = CARTESIAN_POINT ( 'NONE',  ( -13.32578297425849811, 76.85407912984071288, -2.163276995893335997 ) ) ;
#5485 = CARTESIAN_POINT ( 'NONE',  ( -10.71227016036927715, 80.24208485109964784, 8.218659176430634261 ) ) ;
#5486 = CARTESIAN_POINT ( 'NONE',  ( 11.76794919243112325, 14.28000000000000647, 3.823638476888996163 ) ) ;
#5487 = LINE ( 'NONE', #10868, #3834 ) ;
#5488 = CARTESIAN_POINT ( 'NONE',  ( 8.343458848123583849, 4.879999999999997229, -11.48378591275253768 ) ) ;
#5489 = CARTESIAN_POINT ( 'NONE',  ( 12.50000000000000000, -18.00000000000000355, -9.000000000000001776 ) ) ;
#5490 = CARTESIAN_POINT ( 'NONE',  ( 9.520470885617715595, 5.129999999999995453, 6.917026985038135400 ) ) ;
#5491 = CARTESIAN_POINT ( 'NONE',  ( 11.76794919243112325, 49.28000000000000114, 3.823638476888997051 ) ) ;
#5492 = CARTESIAN_POINT ( 'NONE',  ( -11.37499999999960387, -57.23437499999987921, -4.711679271994910323 ) ) ;
#5493 = LINE ( 'NONE', #9305, #2293 ) ;
#5494 = CARTESIAN_POINT ( 'NONE',  ( -13.49999999999999822, -12.92000000000000171, 4.386415899144235908 ) ) ;
#5495 = CARTESIAN_POINT ( 'NONE',  ( -5.651595557928720481, 40.38528827607240856, -12.26012243411721414 ) ) ;
#5496 = CARTESIAN_POINT ( 'NONE',  ( 8.343458848123583849, 35.87999999999999545, -11.48378591275253768 ) ) ;
#5497 = CARTESIAN_POINT ( 'NONE',  ( 13.32852092168753444, 75.35474669015187033, 2.144890943754141688 ) ) ;
#5498 = CARTESIAN_POINT ( 'NONE',  ( 14.25373764215627226, 2.881527793022514356E-15, -11.25789203224866064 ) ) ;
#5499 = CARTESIAN_POINT ( 'NONE',  ( -11.76794919243112325, 32.77999999999999403, -3.823638476888998827 ) ) ;
#5500 = CARTESIAN_POINT ( 'NONE',  ( -9.311494743582063194, 41.31572317635779257, 9.774769270546801891 ) ) ;
#5501 = EDGE_CURVE ( 'NONE', #5168, #4872, #2903, .T. ) ;
#5502 = CARTESIAN_POINT ( 'NONE',  ( -10.46166914714195251, 58.60362355544496182, -8.535617357307549113 ) ) ;
#5503 = CARTESIAN_POINT ( 'NONE',  ( 0.000000000000000000, 3.999999999999961808, -13.50000000000000000 ) ) ;
#5504 = LINE ( 'NONE', #2818, #2131 ) ;
#5505 = CARTESIAN_POINT ( 'NONE',  ( 9.265344266068700207, 30.04200008453489090, 9.818925412339686076 ) ) ;
#5506 = CARTESIAN_POINT ( 'NONE',  ( -25.42428528562860990, 5.918584287042170544, 5.441113646577212748 ) ) ;
#5507 = CARTESIAN_POINT ( 'NONE',  ( -11.19025799215657990, 49.64609340414283878, -7.551709246331172132 ) ) ;
#5508 = CARTESIAN_POINT ( 'NONE',  ( 13.46290329342287961, 63.39539363581478426, 1.002166455802397937 ) ) ;
#5509 = CARTESIAN_POINT ( 'NONE',  ( 11.14094309903787661, 42.14309538808735311, 7.629476624620709302 ) ) ;
#5510 = CARTESIAN_POINT ( 'NONE',  ( -18.99999999999998224, 7.773118517290098062, -1.732050807569074147 ) ) ;
#5511 = EDGE_LOOP ( 'NONE', ( #11856, #16023, #1463, #16354, #3049, #10493, #15830, #3515, #11506, #12696, #3188, #14413, #4378, #14436, #6685, #10747, #17345, #1858, #13448, #10744, #6971, #15762, #13829, #15321, #15919, #17055, #1895, #2408, #2654 ) ) ;
#5512 = CARTESIAN_POINT ( 'NONE',  ( -7.416407864998737942, 4.246025403784436492, 10.20780970022447853 ) ) ;
#5513 = CARTESIAN_POINT ( 'NONE',  ( 2.107853069822502790E-14, 31.18000000000000682, -13.50000000000000000 ) ) ;
#5514 = CARTESIAN_POINT ( 'NONE',  ( 8.343458848123583849, 12.88000000000000611, -11.48378591275253768 ) ) ;
#5515 = VERTEX_POINT ( 'NONE', #15322 ) ;
#5516 = AXIS2_PLACEMENT_3D ( 'NONE', #11576, #5028, #2088 ) ;
#5517 = CARTESIAN_POINT ( 'NONE',  ( -10.96290148446646739, 43.63233836037143476, -7.879540134695893983 ) ) ;
#5518 = CARTESIAN_POINT ( 'NONE',  ( -7.499999999999998224, 104.9266221009243907, 8.932545650451682917 ) ) ;
#5519 = CARTESIAN_POINT ( 'NONE',  ( 11.39486570637464524, 60.70084465595979140, -7.240720970025911640 ) ) ;
#5520 = CARTESIAN_POINT ( 'NONE',  ( 8.343458848123583849, 7.880000000000003446, -11.48378591275253768 ) ) ;
#5521 = CARTESIAN_POINT ( 'NONE',  ( 9.772396245993814290, 72.06742462017868434, 9.313983778355371612 ) ) ;
#5522 = CARTESIAN_POINT ( 'NONE',  ( 13.21191709738701547, 66.52910010606868241, -2.802833979466235359 ) ) ;
#5523 = CARTESIAN_POINT ( 'NONE',  ( 4.938667887072522689, 56.85812260315885425, 12.56421927770909441 ) ) ;
#5524 = CARTESIAN_POINT ( 'NONE',  ( 9.520470885617715595, 73.12999999999999545, 6.917026985038134512 ) ) ;
#5525 = CARTESIAN_POINT ( 'NONE',  ( 3.636496289402154414, 63.82999999999999829, 11.19198476289190936 ) ) ;
#5526 = CARTESIAN_POINT ( 'NONE',  ( -5.721591114156050928, 47.47194874911851770, 12.23566511108304944 ) ) ;
#5527 = DIRECTION ( 'NONE',  ( 0.000000000000000000, 1.000000000000000000, 0.000000000000000000 ) ) ;
#5528 = CARTESIAN_POINT ( 'NONE',  ( 13.50000000000000000, 74.42999999999999261, 1.653273178848926867E-15 ) ) ;
#5529 = CARTESIAN_POINT ( 'NONE',  ( 17.03726630776091611, -100.0000000000000142, 7.069965795335503955 ) ) ;
#5530 = CARTESIAN_POINT ( 'NONE',  ( -4.950837632938861255, 56.50144079815311215, 12.56439702090226795 ) ) ;
#5531 = CARTESIAN_POINT ( 'NONE',  ( -11.37500000000039613, -92.61562499999978115, 4.711679271993002516 ) ) ;
#5532 = CARTESIAN_POINT ( 'NONE',  ( -2.138189944381240881, 52.60311857767972299, 13.49999999999999822 ) ) ;
#5533 = CARTESIAN_POINT ( 'NONE',  ( 11.30035725208420416, 33.70704868103326390, -7.386062474298981329 ) ) ;
#5534 = CARTESIAN_POINT ( 'NONE',  ( -7.999999999999741540, 7.170708369609773314, -19.79695994079638055 ) ) ;
#5535 = CARTESIAN_POINT ( 'NONE',  ( -8.891200544363830713E-16, 70.68000000000000682, 13.50000000000000000 ) ) ;
#5536 = CARTESIAN_POINT ( 'NONE',  ( 7.272992578804311492, 23.88000000000000966, -10.01041549318726709 ) ) ;
#5537 = ORIENTED_EDGE ( 'NONE', *, *, #8764, .T. ) ;
#5538 = CARTESIAN_POINT ( 'NONE',  ( -5.383880044892523031, 62.48502448089114125, 12.38026817833133464 ) ) ;
#5539 = ORIENTED_EDGE ( 'NONE', *, *, #14268, .T. ) ;
#5540 = CARTESIAN_POINT ( 'NONE',  ( -13.48341350937561245, 40.95312764241855774, 0.6709278542534650169 ) ) ;
#5541 = CARTESIAN_POINT ( 'NONE',  ( -7.409984580736203970E-16, -13.32000000000000028, 12.37355403259654985 ) ) ;
#5542 = CARTESIAN_POINT ( 'NONE',  ( 18.62500000000064659, -41.59062499999991758, -7.714727599197336083 ) ) ;
#5543 = EDGE_CURVE ( 'NONE', #12977, #11811, #1894, .T. ) ;
#5544 = CARTESIAN_POINT ( 'NONE',  ( -13.25475736232484536, 44.02032189088402703, 2.561673765456097929 ) ) ;
#5545 = CARTESIAN_POINT ( 'NONE',  ( -7.499999999999995559, -25.08439332921293285, 8.253836299850743075 ) ) ;
#5546 = CARTESIAN_POINT ( 'NONE',  ( 13.50000000000000000, 42.42999999999999261, 1.653273178848926867E-15 ) ) ;
#5547 = CARTESIAN_POINT ( 'NONE',  ( -10.92172942406178926, 48.63000000000000256, -7.935100905948389460 ) ) ;
#5548 = CARTESIAN_POINT ( 'NONE',  ( -13.45742039876322593, 70.96712778246572384, 1.071852073170212583 ) ) ;
#5549 = VECTOR ( 'NONE', #2122, 1000.000000000000000 ) ;
#5550 = CARTESIAN_POINT ( 'NONE',  ( -13.16986379959834252, -15.64374999999994387, -13.16986379960055409 ) ) ;
#5551 = CARTESIAN_POINT ( 'NONE',  ( -6.904622430831049762, 67.43546043278743696, -11.61287708378492844 ) ) ;
#5552 = CARTESIAN_POINT ( 'NONE',  ( -18.62500000000000000, -84.32499999999977547, -1.562973063126292757E-12 ) ) ;
#5553 = CARTESIAN_POINT ( 'NONE',  ( 13.07586280307878646, 54.31047242261610819, 3.357496143552672230 ) ) ;
#5554 = CARTESIAN_POINT ( 'NONE',  ( -11.72818448617283060, 64.68162745856044182, -6.687357485148088365 ) ) ;
#5555 = ORIENTED_EDGE ( 'NONE', *, *, #8842, .F. ) ;
#5556 = CARTESIAN_POINT ( 'NONE',  ( 15.50190989971479816, 7.815224736851132725, -10.85009556066090930 ) ) ;
#5557 = CARTESIAN_POINT ( 'NONE',  ( -11.99508897926147633, 34.70129772595861795, -6.199144905531880134 ) ) ;
#5558 = ORIENTED_EDGE ( 'NONE', *, *, #13733, .F. ) ;
#5559 = CARTESIAN_POINT ( 'NONE',  ( 13.47351438217874353, 78.45921297451653231, -0.8456703420030140528 ) ) ;
#5560 = CARTESIAN_POINT ( 'NONE',  ( -13.35138662365028317, 1.798999282680476490E-09, 1.996909364337476678 ) ) ;
#5561 = AXIS2_PLACEMENT_3D ( 'NONE', #13978, #5797, #9954 ) ;
#5562 = CARTESIAN_POINT ( 'NONE',  ( -8.613042784256499829, 31.51074471318071701, -10.39969252900315588 ) ) ;
#5563 = CARTESIAN_POINT ( 'NONE',  ( 10.39863764822032799, 72.75946676389163770, -8.609374654801005278 ) ) ;
#5564 = CARTESIAN_POINT ( 'NONE',  ( 11.76794919243112680, -9.419999999999999929, -3.823638476888993942 ) ) ;
#5565 = FACE_OUTER_BOUND ( 'NONE', #12257, .T. ) ;
#5566 = CARTESIAN_POINT ( 'NONE',  ( 13.50000000000000355, -16.42000000000000171, -4.386415899144233244 ) ) ;
#5567 = CARTESIAN_POINT ( 'NONE',  ( -8.343458848123576743, 70.48000000000000398, -11.48378591275254301 ) ) ;
#5568 = CARTESIAN_POINT ( 'NONE',  ( -13.22220161272585415, 53.02624049857811883, 2.725156051118921674 ) ) ;
#5569 = CARTESIAN_POINT ( 'NONE',  ( -3.636496289402153081, 44.32999999999999829, -11.19198476289190936 ) ) ;
#5570 = CARTESIAN_POINT ( 'NONE',  ( 13.49999999999999822, 68.28000000000001535, 4.386415899144237684 ) ) ;
#5571 = CARTESIAN_POINT ( 'NONE',  ( -15.67790026899612954, 8.062143948122718839, -8.845307762532401696 ) ) ;
#5572 = CARTESIAN_POINT ( 'NONE',  ( 12.08458693532313077, 69.65149262053893153, -6.018661980718448490 ) ) ;
#5573 = VECTOR ( 'NONE', #11634, 1000.000000000000000 ) ;
#5574 = CARTESIAN_POINT ( 'NONE',  ( -4.329460928816934562, 37.33568557241510177, -12.78734651434877279 ) ) ;
#5575 = CARTESIAN_POINT ( 'NONE',  ( 3.187467471045011269, 35.79457724241678562, 13.12592493638926605 ) ) ;
#5576 = CARTESIAN_POINT ( 'NONE',  ( 1.561832610794586740E-12, -44.71249999999991331, -18.62500000000000000 ) ) ;
#5577 = CARTESIAN_POINT ( 'NONE',  ( -10.42895341926080732, 74.25780691452938242, 8.572557870554565085 ) ) ;
#5578 =( BOUNDED_CURVE ( )  B_SPLINE_CURVE ( 1, ( #5922, #11132 ),
 .UNSPECIFIED., .F., .F. ) 
 B_SPLINE_CURVE_WITH_KNOTS ( ( 2, 2 ),
 ( 0.000000000000000000, 1.000000000000000000 ),
 .UNSPECIFIED. ) 
 CURVE ( )  GEOMETRIC_REPRESENTATION_ITEM ( )  RATIONAL_B_SPLINE_CURVE ( ( 0.9782075447827165426, 0.9782075447827165426 ) ) 
 REPRESENTATION_ITEM ( '' )  );
#5579 = CARTESIAN_POINT ( 'NONE',  ( -12.98389310290256837, 77.06248361752962239, 3.703783162427040754 ) ) ;
#5580 = DIRECTION ( 'NONE',  ( 0.000000000000000000, 0.000000000000000000, 1.000000000000000000 ) ) ;
#5581 = CARTESIAN_POINT ( 'NONE',  ( -15.58845726811976817, 0.000000000000000000, -11.00000000000018296 ) ) ;
#5582 = CARTESIAN_POINT ( 'NONE',  ( -8.711848673609697613, 80.93000000000002103, 8.870066681586113333 ) ) ;
#5583 = DIRECTION ( 'NONE',  ( 1.000000000000000000, 0.000000000000000000, 8.379555213223522577E-14 ) ) ;
#5584 = CARTESIAN_POINT ( 'NONE',  ( -9.520470885617717371, -1.769999999999993801, 6.917026985038133624 ) ) ;
#5585 = ADVANCED_FACE ( 'NONE', ( #2237 ), #16837, .F. ) ;
#5586 = CARTESIAN_POINT ( 'NONE',  ( 9.520470885617715595, 49.13000000000000256, 6.917026985038134512 ) ) ;
#5587 = CARTESIAN_POINT ( 'NONE',  ( -10.92172942406178926, -16.36999999999999744, -7.935100905948389460 ) ) ;
#5588 = CARTESIAN_POINT ( 'NONE',  ( -11.89602199667058535, 40.69392324594991805, -6.382374777626396600 ) ) ;
#5589 = LINE ( 'NONE', #10968, #15029 ) ;
#5590 = CARTESIAN_POINT ( 'NONE',  ( 10.10331317266893336, 75.08473884772422480, 8.954271362371356346 ) ) ;
#5591 = CARTESIAN_POINT ( 'NONE',  ( 17.66377679222614105, 1.677322744816953610E-15, -5.628563848745853804 ) ) ;
#5592 = CARTESIAN_POINT ( 'NONE',  ( -3.636496289402153081, 35.32999999999999829, -11.19198476289190936 ) ) ;
#5593 = CARTESIAN_POINT ( 'NONE',  ( -7.024337696613344839, 41.41931987901391921, 11.52861112765396889 ) ) ;
#5594 = CARTESIAN_POINT ( 'NONE',  ( -3.973104663489275712, 58.32285798913706287, -12.90221010763657361 ) ) ;
#5595 = CYLINDRICAL_SURFACE ( 'NONE', #15765, 2.000000000000001776 ) ;
#5596 = DIRECTION ( 'NONE',  ( 0.000000000000000000, 0.000000000000000000, -1.000000000000000000 ) ) ;
#5597 = CARTESIAN_POINT ( 'NONE',  ( -10.92172942406178926, 57.63000000000000256, -7.935100905948389460 ) ) ;
#5598 = CARTESIAN_POINT ( 'NONE',  ( -13.26588416208786647, 49.84179529059223768, -2.503281531231600798 ) ) ;
#5599 = CARTESIAN_POINT ( 'NONE',  ( 13.49885676942609614, 63.44608529167037858, -0.4713237517850633052 ) ) ;
#5600 = CARTESIAN_POINT ( 'NONE',  ( 10.07256217038269064, 42.08276731119590153, 8.999075269577950564 ) ) ;
#5601 = CARTESIAN_POINT ( 'NONE',  ( 1.747925173837019175, 38.74284411846687703, 13.38730336300498536 ) ) ;
#5602 = ORIENTED_EDGE ( 'NONE', *, *, #16490, .F. ) ;
#5603 = CARTESIAN_POINT ( 'NONE',  ( -4.225622128461934857, 70.33197010581022823, -12.82179701616371226 ) ) ;
#5604 = CARTESIAN_POINT ( 'NONE',  ( 8.043339635997654113, -18.73124999999995666, -8.043339635996304082 ) ) ;
#5605 = CARTESIAN_POINT ( 'NONE',  ( -8.549982208541774191E-16, 17.68000000000001748, 14.19474002721660355 ) ) ;
#5606 = ORIENTED_EDGE ( 'NONE', *, *, #3449, .F. ) ;
#5607 = ADVANCED_FACE ( 'NONE', ( #4741 ), #10145, .T. ) ;
#5608 = CARTESIAN_POINT ( 'NONE',  ( -6.508780211867530419, 43.41933150643208705, -11.83743217236817102 ) ) ;
#5609 = CARTESIAN_POINT ( 'NONE',  ( -7.499999999999999112, 108.6686507028258717, -2.034160311361953966 ) ) ;
#5610 = CARTESIAN_POINT ( 'NONE',  ( 10.70400462187975776, 60.74250492953063230, -8.227714730520327535 ) ) ;
#5611 = CARTESIAN_POINT ( 'NONE',  ( 8.343458848123583849, 13.87999999999999012, -11.48378591275253768 ) ) ;
#5612 = CARTESIAN_POINT ( 'NONE',  ( -12.00000000000000178, 6.796025403784443419, -2.718289652585035561E-15 ) ) ;
#5613 = CARTESIAN_POINT ( 'NONE',  ( 13.49854170867679493, 66.44634207941858506, -0.4798613340506648894 ) ) ;
#5614 = CARTESIAN_POINT ( 'NONE',  ( 6.439080603729475882, 56.91648054290170222, 11.87284769991120648 ) ) ;
#5615 = CARTESIAN_POINT ( 'NONE',  ( -9.520470885617715595, 59.63000000000000256, -6.917026985038136289 ) ) ;
#5616 = CARTESIAN_POINT ( 'NONE',  ( 3.636496289402157078, 68.03000000000000114, -11.19198476289190936 ) ) ;
#5617 = CARTESIAN_POINT ( 'NONE',  ( -9.668289202133056648, 47.29798508749041019, 9.423919283597269825 ) ) ;
#5618 = CARTESIAN_POINT ( 'NONE',  ( -4.171729424061787483, 45.33000000000000540, -12.83926296998457417 ) ) ;
#5619 = DIRECTION ( 'NONE',  ( 0.000000000000000000, -1.000000000000000000, 0.000000000000000000 ) ) ;
#5620 = CARTESIAN_POINT ( 'NONE',  ( 4.371733802976720540, -100.0000000000000000, 15.22508764378929058 ) ) ;
#5621 = TOROIDAL_SURFACE ( 'NONE', #13499, 6.000000000000001776, 6.000000000000000000 ) ;
#5622 = CARTESIAN_POINT ( 'NONE',  ( -10.40911334466800575, 10.00000000000000178, -6.687738405650081930 ) ) ;
#5623 = CARTESIAN_POINT ( 'NONE',  ( 11.37500000000000000, -83.24999999999980105, 9.531744055041752924E-13 ) ) ;
#5624 = CARTESIAN_POINT ( 'NONE',  ( -8.891200544363830713E-16, 5.680000000000002380, 13.49999999999999822 ) ) ;
#5625 = CARTESIAN_POINT ( 'NONE',  ( 13.01499335373094013, 33.55803638891549667, -3.586594114771764374 ) ) ;
#5626 = CARTESIAN_POINT ( 'NONE',  ( -0.7873830781139755652, 9.999999999999998224, 12.87957660135147542 ) ) ;
#5627 = DIRECTION ( 'NONE',  ( 0.000000000000000000, -1.000000000000000000, 0.000000000000000000 ) ) ;
#5628 = ORIENTED_EDGE ( 'NONE', *, *, #11125, .T. ) ;
#5629 = DIRECTION ( 'NONE',  ( -1.000000000000000000, -1.301042606982605567E-16, -0.000000000000000000 ) ) ;
#5630 = ORIENTED_EDGE ( 'NONE', *, *, #7310, .T. ) ;
#5631 = EDGE_CURVE ( 'NONE', #16216, #14697, #10548, .T. ) ;
#5632 = CARTESIAN_POINT ( 'NONE',  ( -7.714727599197334307, -62.40312499999986073, -18.62500000000064659 ) ) ;
#5633 = CARTESIAN_POINT ( 'NONE',  ( -13.47827025046990990, 43.95642512897427423, 0.7656873746960646265 ) ) ;
#5634 = CARTESIAN_POINT ( 'NONE',  ( -10.35602470258073105, 7.924935932049796072, 15.34492079894888050 ) ) ;
#5635 = VECTOR ( 'NONE', #5663, 1000.000000000000000 ) ;
#5636 = CARTESIAN_POINT ( 'NONE',  ( -8.343458848123582072, 38.37999999999998835, 11.48378591275254124 ) ) ;
#5637 = CARTESIAN_POINT ( 'NONE',  ( -4.171729424061791036, 46.53000000000000114, 12.83926296998457239 ) ) ;
#5638 = CARTESIAN_POINT ( 'NONE',  ( -12.81710173804216346, 71.08258523398228590, 4.240278988823360962 ) ) ;
#5639 = CARTESIAN_POINT ( 'NONE',  ( -13.16986379960055409, -19.80624999999993463, 13.16986379959834252 ) ) ;
#5640 = CARTESIAN_POINT ( 'NONE',  ( -11.73022876284554883, 67.68182808645379112, -6.682201463345557535 ) ) ;
#5641 = CARTESIAN_POINT ( 'NONE',  ( -1.564113515457998370E-12, -71.83749999999979252, 18.62500000000000000 ) ) ;
#5642 = CARTESIAN_POINT ( 'NONE',  ( 11.67482575541059475, 54.17791662511717732, 6.778571967042572588 ) ) ;
#5643 = CIRCLE ( 'NONE', #17473, 14.50000000000000000 ) ;
#5644 = CARTESIAN_POINT ( 'NONE',  ( -3.261899838592319689, 64.29728490861971579, -13.10000070067140321 ) ) ;
#5645 = ORIENTED_EDGE ( 'NONE', *, *, #4272, .F. ) ;
#5646 = CARTESIAN_POINT ( 'NONE',  ( -13.49999999999999822, 64.07999999999999829, 4.386415899144235020 ) ) ;
#5647 = CARTESIAN_POINT ( 'NONE',  ( -12.51102511793943961, 34.74498775374014059, -5.090906052585752128 ) ) ;
#5648 = EDGE_LOOP ( 'NONE', ( #17251, #927, #13574, #4084 ) ) ;
#5649 = CARTESIAN_POINT ( 'NONE',  ( 13.49994509081106386, 78.41450604159769000, 0.4393232071407982553 ) ) ;
#5650 = CARTESIAN_POINT ( 'NONE',  ( 7.499999999999996447, -8.000000000000000000, -9.367496997597600128 ) ) ;
#5651 = DIRECTION ( 'NONE',  ( -0.000000000000000000, 1.000000000000000000, -0.000000000000000000 ) ) ;
#5652 = CARTESIAN_POINT ( 'NONE',  ( 11.18757194939378330, 72.71406989031071078, -7.555694557022631486 ) ) ;
#5653 = CARTESIAN_POINT ( 'NONE',  ( 12.50000000000000000, -18.00000000000000355, -2.204364238465235822E-15 ) ) ;
#5654 = CARTESIAN_POINT ( 'NONE',  ( 2.621994543952811015E-15, -18.81999999999999673, -14.19474002721660355 ) ) ;
#5655 = CARTESIAN_POINT ( 'NONE',  ( 13.50000000000000000, 75.42999999999999261, 1.653273178848926867E-15 ) ) ;
#5656 = CARTESIAN_POINT ( 'NONE',  ( -11.42382290241512521, 52.66093731307155679, -7.194032250886600366 ) ) ;
#5657 = CARTESIAN_POINT ( 'NONE',  ( 11.76794919243112680, 43.57999999999999119, -3.823638476888993942 ) ) ;
#5658 = CARTESIAN_POINT ( 'NONE',  ( -8.691771469529815392E-16, 70.67999999999999261, 14.19474002721660355 ) ) ;
#5659 = DIRECTION ( 'NONE',  ( 0.000000000000000000, 0.000000000000000000, -1.000000000000000000 ) ) ;
#5660 = B_SPLINE_CURVE_WITH_KNOTS ( 'NONE', 3,
 ( #5765, #11149, #8422, #15273, #16525, #13775, #15185, #1674, #4518, #15447, #16436, #13949, #9839, #4338, #1764, #11413, #12643, #8512, #532, #3172, #7259, #7353, #1846, #16700, #7173, #8683, #447, #16785, #4605, #3266, #14042, #1930, #3356, #8772, #7006, #9748, #15092, #14298, #4862, #15797, #12904, #17221, #5131, #10522, #14381, #16873, #17045, #14212, #960, #2271, #12988, #6372, #707, #15532, #11584, #4950, #13162, #788, #10265, #6117, #15885, #11846, #4778, #12820, #11497, #6198, #1048, #2358, #3612, #6461, #7612, #7440, #2013, #8940, #11756, #15616, #5042, #3443, #871, #10354, #16960, #6282, #17132, #7524, #9205, #11670, #15708, #10181, #8858, #9026, #2097, #3525, #2184, #10439, #7697, #13074, #3703, #3792, #9120, #14470, #7791, #10956, #14644, #10775, #11926, #8045, #10606, #6633, #2616, #6898, #13413, #7872, #13249, #2796, #3876, #14557, #9292, #2532, #17307, #17477, #2440, #12183, #4050, #15973, #7960, #5219, #16230, #16140, #13330, #14811, #3965, #16058, #1221, #12013, #9463, #74, #1136, #6547, #17393, #2706, #9552, #10861, #5309, #10692, #9378, #5390, #14727, #1303, #6717, #12095, #14902, #8135, #5480, #13500, #1390, #6805, #4139, #8227, #12272, #16324, #13588, #1482, #169, #5574, #4230, #9907, #8492, #4318, #16505, #12542, #14023, #16592, #15254, #15074, #13843, #3153, #9728, #7071, #15343, #8404, #12362, #7157, #1656 ),
 .UNSPECIFIED., .F., .F.,
 ( 4, 2, 1, 2, 2, 1, 2, 2, 2, 2, 1, 1, 2, 2, 1, 2, 2, 2, 2, 2, 1, 2, 2, 1, 1, 2, 2, 1, 2, 2, 2, 2, 1, 1, 1, 2, 2, 2, 1, 1, 2, 2, 1, 2, 2, 2, 2, 1, 2, 2, 1, 2, 2, 2, 1, 1, 2, 2, 2, 2, 2, 2, 2, 2, 2, 2, 2, 2, 2, 1, 1, 1, 2, 2, 1, 1, 1, 2, 2, 2, 2, 2, 2, 1, 2, 2, 1, 2, 2, 2, 1, 2, 2, 1, 2, 2, 2, 2, 1, 1, 1, 1, 2, 2, 2, 2, 2, 4 ),
 ( 0.8284411291432991487, 0.8293602319378399201, 0.8294751197871574888, 0.8295038417494868810, 0.8295325637118162732, 0.8295900076364750575, 0.8298197833351103059, 0.8302793347323806916, 0.8311984375269214631, 0.8314282132255567115, 0.8314856571502154958, 0.8315143791125448880, 0.8315287400937095841, 0.8315431010748742802, 0.8316579889241918488, 0.8321175403214622346, 0.8330366431160030061, 0.8334961945132733918, 0.8335536384379321762, 0.8336110823625909605, 0.8337259702119086402, 0.8339557459105437776, 0.8348748487050845490, 0.8353344001023548238, 0.8355641758009900721, 0.8355928977633194643, 0.8356216197256488565, 0.8356790636503076408, 0.8357939514996252095, 0.8367130542941659810, 0.8371726056914362557, 0.8374023813900715041, 0.8375172692393890728, 0.8375747131640478571, 0.8376034351263772493, 0.8376177961075419454, 0.8376321570887066414, 0.8394703626777877403, 0.8395852505271053090, 0.8396426944517640933, 0.8396570554329287894, 0.8396714164140934855, 0.8397001383764228777, 0.8399299140750580150, 0.8403894654723281787, 0.8413085682668687282, 0.8415383439655038655, 0.8416532318148214342, 0.8416819537771508264, 0.8417106757394802186, 0.8417681196641390029, 0.8422276710614091666, 0.8431467738559497160, 0.8436063252532199908, 0.8436637691778787751, 0.8436924911402081673, 0.8437068521213728634, 0.8437212131025375594, 0.8438361009518551281, 0.8440658766504902655, 0.8449849794450308149, 0.8454445308423010896, 0.8456743065409362270, 0.8457891943902537957, 0.8459040822395713644, 0.8468231850341118028, 0.8477422878286523522, 0.8477710097909817444, 0.8477997317533111366, 0.8478571756779699209, 0.8479720635272874896, 0.8482018392259226269, 0.8486613906231930127, 0.8495804934177335621, 0.8496953812670511308, 0.8497528251917099151, 0.8497815471540393073, 0.8497959081352040034, 0.8498102691163686995, 0.8500400448150039479, 0.8504995962122743336, 0.8514186990068152161, 0.8516484747054503535, 0.8517633625547680332, 0.8518208064794268175, 0.8518495284417562097, 0.8518782504040856018, 0.8523378018013559876, 0.8532569045958968701, 0.8537164559931672558, 0.8538313438424848245, 0.8538600658048142167, 0.8538887877671437199, 0.8539462316918025042, 0.8541760073904376416, 0.8546355587877080273, 0.8548653344863431647, 0.8549802223356608444, 0.8550951101849784131, 0.8555546615822487988, 0.8557844372808839362, 0.8558418812055427205, 0.8558706031678721127, 0.8558993251302015048, 0.8560142129795191845, 0.8569333157740598450, 0.8573928671713302307, 0.8578524185686006165 ),
 .UNSPECIFIED. ) ;
#5661 = EDGE_CURVE ( 'NONE', #3933, #4554, #2065, .T. ) ;
#5662 = CARTESIAN_POINT ( 'NONE',  ( 3.582496635403904062, 68.80879950270664835, 13.01598647554185639 ) ) ;
#5663 = DIRECTION ( 'NONE',  ( 0.000000000000000000, -1.000000000000000000, 0.000000000000000000 ) ) ;
#5664 = AXIS2_PLACEMENT_3D ( 'NONE', #7318, #2158, #11382 ) ;
#5665 = CARTESIAN_POINT ( 'NONE',  ( 9.708203932499371192, 5.596025403784450347, -7.053423027509677645 ) ) ;
#5666 = CARTESIAN_POINT ( 'NONE',  ( -13.16986379959834252, -46.79374999999990337, -13.16986379960055409 ) ) ;
#5667 = CARTESIAN_POINT ( 'NONE',  ( -11.99020945619393075, 74.15891743954519200, 6.203620012955681773 ) ) ;
#5668 = CARTESIAN_POINT ( 'NONE',  ( -5.437383120998211972, 76.37690954485367456, -12.36259108923011674 ) ) ;
#5669 = CARTESIAN_POINT ( 'NONE',  ( 24.73863375370592976, 5.918584287042170544, 8.000000000000106581 ) ) ;
#5670 = LINE ( 'NONE', #345, #10058 ) ;
#5671 = DIRECTION ( 'NONE',  ( 0.000000000000000000, 0.000000000000000000, 1.000000000000000000 ) ) ;
#5672 = DIRECTION ( 'NONE',  ( 0.000000000000000000, 0.000000000000000000, -1.000000000000000000 ) ) ;
#5673 = CARTESIAN_POINT ( 'NONE',  ( 7.272992578804311492, -9.120000000000004547, -10.01041549318726709 ) ) ;
#5674 = CARTESIAN_POINT ( 'NONE',  ( 11.76794919243112680, 46.57999999999999829, -3.823638476888993942 ) ) ;
#5675 = CARTESIAN_POINT ( 'NONE',  ( 13.50000000000000000, -14.57000000000000028, 1.734723475976807094E-15 ) ) ;
#5676 = CARTESIAN_POINT ( 'NONE',  ( -10.40732797419851963, 32.25961365229549926, 8.610261354245384524 ) ) ;
#5677 = CARTESIAN_POINT ( 'NONE',  ( 13.48494557894230539, 75.45196395580148874, -0.6373953516020099963 ) ) ;
#5678 = CARTESIAN_POINT ( 'NONE',  ( 3.972737467449376503, -1.623771540364909428E-16, -13.12643016014658848 ) ) ;
#5679 = CARTESIAN_POINT ( 'NONE',  ( -11.76794919243112325, 33.07999999999998408, 3.823638476888994386 ) ) ;
#5680 = CARTESIAN_POINT ( 'NONE',  ( -12.53918026858758061, 41.11172392978211576, 5.001923395695291319 ) ) ;
#5681 =( GEOMETRIC_REPRESENTATION_CONTEXT ( 3 ) GLOBAL_UNCERTAINTY_ASSIGNED_CONTEXT ( ( #10004 ) ) GLOBAL_UNIT_ASSIGNED_CONTEXT ( ( #15008, #12290, #16433 ) ) REPRESENTATION_CONTEXT ( 'NONE', 'WORKASPACE' ) );
#5682 = CARTESIAN_POINT ( 'NONE',  ( 4.861248255796603246, 52.00477046739004550, -12.59468897525855624 ) ) ;
#5683 = ADVANCED_FACE ( 'NONE', ( #3578 ), #3493, .T. ) ;
#5684 = DIRECTION ( 'NONE',  ( -1.000000000000000000, -0.000000000000000000, -0.000000000000000000 ) ) ;
#5685 = CARTESIAN_POINT ( 'NONE',  ( 8.293271311656841505, 36.86388732214020081, -10.65232149131729855 ) ) ;
#5686 = DIRECTION ( 'NONE',  ( 0.000000000000000000, -1.000000000000000000, 0.000000000000000000 ) ) ;
#5687 = CARTESIAN_POINT ( 'NONE',  ( -13.36307422868558703, 49.86276556841097118, -1.922284815108510792 ) ) ;
#5688 = CARTESIAN_POINT ( 'NONE',  ( 10.61938128423869365, 63.11274346617898345, 8.335457914628065623 ) ) ;
#5689 = CARTESIAN_POINT ( 'NONE',  ( 8.359408846421068517, 41.99913092812320059, 10.60054140072220008 ) ) ;
#5690 = CARTESIAN_POINT ( 'NONE',  ( 4.140633560867821750, 38.82887436838161932, 12.84970033327834926 ) ) ;
#5691 = ORIENTED_EDGE ( 'NONE', *, *, #10327, .T. ) ;
#5692 = CARTESIAN_POINT ( 'NONE',  ( -9.520470885617717371, 72.23000000000000398, 6.917026985038133624 ) ) ;
#5693 = CARTESIAN_POINT ( 'NONE',  ( 10.00000000000002132, 0.000000000000000000, -17.32050807568876394 ) ) ;
#5694 = CARTESIAN_POINT ( 'NONE',  ( 8.043339635996300530, -47.86874999999988489, 8.043339635997654113 ) ) ;
#5695 = VERTEX_POINT ( 'NONE', #5100 ) ;
#5696 = CARTESIAN_POINT ( 'NONE',  ( -2.258558314520655141, 43.26120942166914318, -13.30973117251418358 ) ) ;
#5697 = DIRECTION ( 'NONE',  ( -0.000000000000000000, 1.000000000000000000, -0.000000000000000000 ) ) ;
#5698 = CARTESIAN_POINT ( 'NONE',  ( 11.18658721041314763, 60.71407845817507365, -7.562691393858058220 ) ) ;
#5699 = CARTESIAN_POINT ( 'NONE',  ( -8.343458848123582072, 0.3799999999999937317, 11.48378591275254124 ) ) ;
#5700 = DIRECTION ( 'NONE',  ( 0.000000000000000000, 1.000000000000000000, 0.000000000000000000 ) ) ;
#5701 = CARTESIAN_POINT ( 'NONE',  ( 13.39967370095669352, 66.37080031235018396, 1.701620727286339285 ) ) ;
#5702 = CARTESIAN_POINT ( 'NONE',  ( 1.442593713695419444, 56.73187045217319735, 13.42270898593407935 ) ) ;
#5703 = CARTESIAN_POINT ( 'NONE',  ( 9.520470885617715595, 55.12999999999999545, 6.917026985038134512 ) ) ;
#5704 = CARTESIAN_POINT ( 'NONE',  ( -7.576616670048093940E-16, 69.68000000000000682, 12.37355403259654985 ) ) ;
#5705 = CARTESIAN_POINT ( 'NONE',  ( -13.49176311494470681, 46.94621656216333605, 0.4715414884418810404 ) ) ;
#5706 = CARTESIAN_POINT ( 'NONE',  ( 0.000000000000000000, 0.000000000000000000, 0.000000000000000000 ) ) ;
#5707 = CARTESIAN_POINT ( 'NONE',  ( 2.000520122481862502E-14, 73.67999999999999261, 13.50000000000000000 ) ) ;
#5708 = ADVANCED_FACE ( 'NONE', ( #12782 ), #6167, .F. ) ;
#5709 = CARTESIAN_POINT ( 'NONE',  ( 8.331761120487128025, 30.86213173433371182, -10.62223457817614225 ) ) ;
#5710 = CARTESIAN_POINT ( 'NONE',  ( -5.728624354601031143, 56.47170591170164045, 12.22464376188452206 ) ) ;
#5711 = CARTESIAN_POINT ( 'NONE',  ( -9.552639591052204498E-13, -79.08749999999980673, 11.37500000000000000 ) ) ;
#5712 = CARTESIAN_POINT ( 'NONE',  ( -4.171729424061787483, 51.32999999999999829, -12.83926296998457417 ) ) ;
#5713 = CARTESIAN_POINT ( 'NONE',  ( 9.450540653006603620, 33.05113386618337756, 9.640956752933217189 ) ) ;
#5714 = CARTESIAN_POINT ( 'NONE',  ( 7.575483063523256178, 10.00000000000000000, 11.14317524721867692 ) ) ;
#5715 = CARTESIAN_POINT ( 'NONE',  ( 4.192885926659680962, 40.02925677665264459, -12.83275633162273976 ) ) ;
#5716 = ORIENTED_EDGE ( 'NONE', *, *, #8002, .T. ) ;
#5717 = CARTESIAN_POINT ( 'NONE',  ( -6.180644893164205733, 62.45382428835798549, 12.00516588008592045 ) ) ;
#5718 = ORIENTED_EDGE ( 'NONE', *, *, #11157, .T. ) ;
#5719 = CARTESIAN_POINT ( 'NONE',  ( 18.62500000000000000, -40.54999999999992610, 1.560692158462880521E-12 ) ) ;
#5720 = CARTESIAN_POINT ( 'NONE',  ( -13.42920886623006105, 43.88144049818974679, -1.399576480510955401 ) ) ;
#5721 = VECTOR ( 'NONE', #13877, 1000.000000000000000 ) ;
#5722 = CARTESIAN_POINT ( 'NONE',  ( -8.000000000000140332, 7.815224843475954586, 17.14741290055376410 ) ) ;
#5723 = CARTESIAN_POINT ( 'NONE',  ( 13.49999999999999822, 30.27999999999999403, 4.386415899144237684 ) ) ;
#5724 = EDGE_CURVE ( 'NONE', #106, #13215, #12870, .T. ) ;
#5725 = CARTESIAN_POINT ( 'NONE',  ( -6.333153400715997527, 46.41227267698536707, -11.92229910835860096 ) ) ;
#5726 = CARTESIAN_POINT ( 'NONE',  ( -7.633650000891075038, 67.46670873368714183, -11.13611842294216814 ) ) ;
#5727 = CARTESIAN_POINT ( 'NONE',  ( -13.16986379960055409, -36.45624999999989768, 13.16986379959834252 ) ) ;
#5728 = VECTOR ( 'NONE', #17092, 1000.000000000000000 ) ;
#5729 = CARTESIAN_POINT ( 'NONE',  ( 13.47366810957596073, 54.45994921630894225, -0.8662603028162058072 ) ) ;
#5730 = CARTESIAN_POINT ( 'NONE',  ( -7.473959287627094383, 64.45978679042782744, -11.24528175482741688 ) ) ;
#5731 = ORIENTED_EDGE ( 'NONE', *, *, #16652, .F. ) ;
#5732 = CARTESIAN_POINT ( 'NONE',  ( 15.34211313687880285, 8.027799056124985455, -9.658320279281790377 ) ) ;
#5733 = CARTESIAN_POINT ( 'NONE',  ( -11.84936134568200750, 34.69045658404807142, -6.468588641860953281 ) ) ;
#5734 = ORIENTED_EDGE ( 'NONE', *, *, #2233, .F. ) ;
#5735 = CARTESIAN_POINT ( 'NONE',  ( 11.80121533525529998, 78.18692176761594226, 6.556313531099895897 ) ) ;
#5736 = CARTESIAN_POINT ( 'NONE',  ( 13.49999999999999822, 47.28000000000000114, 4.386415899144236796 ) ) ;
#5737 = CARTESIAN_POINT ( 'NONE',  ( 7.500000000000001776, -25.65291190719445780, -7.723695278929457508 ) ) ;
#5738 = CARTESIAN_POINT ( 'NONE',  ( 9.400174290359263551, 72.81156905856246908, -9.698804889119921668 ) ) ;
#5739 = CARTESIAN_POINT ( 'NONE',  ( 2.473603416425627088, 79.09105862451949065, -13.27151636866100404 ) ) ;
#5740 = CARTESIAN_POINT ( 'NONE',  ( 13.50000000000000000, -13.56999999999999851, 1.734723475976807094E-15 ) ) ;
#5741 = CARTESIAN_POINT ( 'NONE',  ( 2.607531440858944223E-15, 61.17999999999998550, -14.19474002721660355 ) ) ;
#5742 = CARTESIAN_POINT ( 'NONE',  ( -13.46057364109657151, 52.96569535534638362, 1.031020640244758368 ) ) ;
#5743 = CARTESIAN_POINT ( 'NONE',  ( -7.576616670048093940E-16, 39.67999999999999261, 12.37355403259654985 ) ) ;
#5744 = CARTESIAN_POINT ( 'NONE',  ( 9.520470885617717371, -18.27000000000000313, -6.917026985038131848 ) ) ;
#5745 = CARTESIAN_POINT ( 'NONE',  ( 4.171729424061789260, 58.82999999999999829, 12.83926296998457417 ) ) ;
#5746 = CARTESIAN_POINT ( 'NONE',  ( 0.000000000000000000, 3.999999999999961808, 0.000000000000000000 ) ) ;
#5747 = CARTESIAN_POINT ( 'NONE',  ( 12.20035770258772878, 69.21726674062897189, 5.799875816967380082 ) ) ;
#5748 = DIRECTION ( 'NONE',  ( 0.000000000000000000, 1.000000000000000000, 0.000000000000000000 ) ) ;
#5749 = PLANE ( 'NONE',  #11755 ) ;
#5750 = CARTESIAN_POINT ( 'NONE',  ( -18.62500000000000000, -82.17499999999982663, -1.562973063126292757E-12 ) ) ;
#5751 = CARTESIAN_POINT ( 'NONE',  ( -11.28504704467765407, 74.20798629947016423, 7.409300117848043321 ) ) ;
#5752 = CARTESIAN_POINT ( 'NONE',  ( -9.412723707183822341, 76.54928254877205518, -9.677326817764578593 ) ) ;
#5753 = CARTESIAN_POINT ( 'NONE',  ( 10.92172942406178926, 4.129999999999994564, 7.935100905948385908 ) ) ;
#5754 =( NAMED_UNIT ( * ) PLANE_ANGLE_UNIT ( ) SI_UNIT ( $, .RADIAN. ) );
#5755 = CARTESIAN_POINT ( 'NONE',  ( -7.272992578804310604, -10.62000000000000099, 10.01041549318726709 ) ) ;
#5756 = CARTESIAN_POINT ( 'NONE',  ( -3.636496289402153081, 41.32999999999999829, -11.19198476289190936 ) ) ;
#5757 = CARTESIAN_POINT ( 'NONE',  ( -24.73863375370603634, 5.918584287042171432, 7.999999999999761080 ) ) ;
#5758 = CARTESIAN_POINT ( 'NONE',  ( -4.700843871787972361, 32.51074219333796833, 12.65638779739501629 ) ) ;
#5759 = CARTESIAN_POINT ( 'NONE',  ( 13.48116795019819847, 75.45464721144679743, -0.7146242057943285042 ) ) ;
#5760 = EDGE_CURVE ( 'NONE', #5168, #15852, #13129, .T. ) ;
#5761 = CARTESIAN_POINT ( 'NONE',  ( 9.608090060877380267, -7.486575357575243633E-16, -6.851496304736921061 ) ) ;
#5762 = CARTESIAN_POINT ( 'NONE',  ( 3.636496289402154414, 33.82999999999999829, 11.19198476289190936 ) ) ;
#5763 = CARTESIAN_POINT ( 'NONE',  ( 13.50000000000000355, 83.57999999999999829, -4.386415899144233244 ) ) ;
#5764 = CARTESIAN_POINT ( 'NONE',  ( -1.005545769327274827E-13, 52.18000000000000682, -13.50000000000000000 ) ) ;
#5765 = CARTESIAN_POINT ( 'NONE',  ( 1.785599194582236620E-06, 38.68004968046676595, 13.49999999999976374 ) ) ;
#5766 = CARTESIAN_POINT ( 'NONE',  ( 0.1182731081639512155, 37.17574734598938591, -13.49948365268883776 ) ) ;
#5767 = CARTESIAN_POINT ( 'NONE',  ( -3.708203932499374744, 0.4639745962155741310, -11.41267819554187035 ) ) ;
#5768 = CARTESIAN_POINT ( 'NONE',  ( -0.5736229098616415500, 49.20060530840606816, -13.48854776642249576 ) ) ;
#5769 = CARTESIAN_POINT ( 'NONE',  ( 7.569887829306680693, 62.96389870297073088, 11.17971963918203393 ) ) ;
#5770 = CARTESIAN_POINT ( 'NONE',  ( 12.34753929015662521, 42.23053449865343367, 5.457913282602898875 ) ) ;
#5771 = CARTESIAN_POINT ( 'NONE',  ( 6.202863237649241412, 48.95301221118648272, -11.99187382583002126 ) ) ;
#5772 = CARTESIAN_POINT ( 'NONE',  ( 7.272992578804311492, 23.88000000000000966, -10.01041549318726709 ) ) ;
#5773 = ORIENTED_EDGE ( 'NONE', *, *, #6605, .T. ) ;
#5774 = CARTESIAN_POINT ( 'NONE',  ( -9.520470885617715595, 77.63000000000000966, -6.917026985038136289 ) ) ;
#5775 = DIRECTION ( 'NONE',  ( -0.000000000000000000, 1.000000000000000000, -0.000000000000000000 ) ) ;
#5776 = CARTESIAN_POINT ( 'NONE',  ( -11.37500000000000000, -74.92499999999982663, -9.545674412382054647E-13 ) ) ;
#5777 = CARTESIAN_POINT ( 'NONE',  ( 13.50000000000000000, 9.429999999999994387, 1.734723475976807094E-15 ) ) ;
#5778 = EDGE_LOOP ( 'NONE', ( #7124, #13784, #3562, #15834 ) ) ;
#5779 = CARTESIAN_POINT ( 'NONE',  ( -5.664207996239682963, 43.38577903074708075, -12.25425443241694090 ) ) ;
#5780 = CARTESIAN_POINT ( 'NONE',  ( -7.499999999999999112, 102.9299999999999073, -9.367496997597655195 ) ) ;
#5781 = CARTESIAN_POINT ( 'NONE',  ( 7.332788481940905712, 60.90639710865967515, -11.33710643711476251 ) ) ;
#5782 = CARTESIAN_POINT ( 'NONE',  ( -8.343458848123576743, 5.480000000000007532, -11.48378591275254301 ) ) ;
#5783 = CARTESIAN_POINT ( 'NONE',  ( -2.734444271416374749E-11, 0.3139745962166686777, -12.00000000000000000 ) ) ;
#5784 = DIRECTION ( 'NONE',  ( 1.776356839400250465E-15, 0.000000000000000000, 1.000000000000000000 ) ) ;
#5785 = CARTESIAN_POINT ( 'NONE',  ( 9.629085971571848646, 66.06008022608338592, 9.468271534833982983 ) ) ;
#5786 = CARTESIAN_POINT ( 'NONE',  ( 10.66232145652183760, 57.11515599909031238, 8.280407745028306010 ) ) ;
#5787 = CARTESIAN_POINT ( 'NONE',  ( -3.636496289402155746, 57.53000000000000114, 11.19198476289190936 ) ) ;
#5788 = CARTESIAN_POINT ( 'NONE',  ( 8.343458848123578520, 34.97999999999999687, 11.48378591275254124 ) ) ;
#5789 = CARTESIAN_POINT ( 'NONE',  ( 9.520470885617715595, 67.12999999999999545, 6.917026985038134512 ) ) ;
#5790 = CARTESIAN_POINT ( 'NONE',  ( -13.48570619275009008, 46.95166055620521917, 0.6284690211920893610 ) ) ;
#5791 = CARTESIAN_POINT ( 'NONE',  ( 5.912838536822658142, 45.96461575129709587, -12.13792530647693546 ) ) ;
#5792 = CARTESIAN_POINT ( 'NONE',  ( 0.1772876194880554368, 8.062177826491097932, -18.00000000000000355 ) ) ;
#5793 = SURFACE_STYLE_FILL_AREA ( #13804 ) ;
#5794 = CARTESIAN_POINT ( 'NONE',  ( 5.785475118908125047, 30.96942592604588285, -12.19750789377168232 ) ) ;
#5795 = CARTESIAN_POINT ( 'NONE',  ( -5.595416803014888529, 56.47688909101474053, 12.28583926748330590 ) ) ;
#5796 = CARTESIAN_POINT ( 'NONE',  ( -9.552639591052204498E-13, -95.73749999999976978, 11.37500000000000000 ) ) ;
#5797 = DIRECTION ( 'NONE',  ( -1.000000000000000000, -0.000000000000000000, -0.000000000000000000 ) ) ;
#5798 = CIRCLE ( 'NONE', #6074, 4.000000000000000000 ) ;
#5799 = CARTESIAN_POINT ( 'NONE',  ( 12.55310634897202959, 33.24964244554870163, 4.968087426967330522 ) ) ;
#5800 = DIRECTION ( 'NONE',  ( -9.821670480311996085E-15, 0.000000000000000000, 1.000000000000000000 ) ) ;
#5801 = CARTESIAN_POINT ( 'NONE',  ( 0.000000000000000000, 80.93000000000000682, -13.50000000000000000 ) ) ;
#5802 = VERTEX_POINT ( 'NONE', #16924 ) ;
#5803 = CARTESIAN_POINT ( 'NONE',  ( -13.50527712561470040, 61.93091922064468946, 0.03146696456400008973 ) ) ;
#5804 = ORIENTED_EDGE ( 'NONE', *, *, #10758, .F. ) ;
#5805 = CARTESIAN_POINT ( 'NONE',  ( 7.714727599200456254, -76.97187499999985505, -18.62499999999935341 ) ) ;
#5806 = EDGE_CURVE ( 'NONE', #4640, #7799, #669, .T. ) ;
#5807 = CARTESIAN_POINT ( 'NONE',  ( -11.26318954741650735, 44.20936586529614232, 7.442652888113295617 ) ) ;
#5808 = ADVANCED_FACE ( 'NONE', ( #14091, #4827 ), #6082, .F. ) ;
#5809 = FACE_OUTER_BOUND ( 'NONE', #6064, .T. ) ;
#5810 = CARTESIAN_POINT ( 'NONE',  ( 10.92172942406179104, 36.72999999999999687, -7.935100905948385908 ) ) ;
#5811 = CARTESIAN_POINT ( 'NONE',  ( 2.607531440858944223E-15, 48.17999999999999261, -14.19474002721660355 ) ) ;
#5812 = CARTESIAN_POINT ( 'NONE',  ( -0.3591556296474884835, 46.19290918421699388, -13.49539728357718182 ) ) ;
#5813 = CARTESIAN_POINT ( 'NONE',  ( -2.933613647220042697, 67.28548860721471669, -13.17740267288178480 ) ) ;
#5814 = CARTESIAN_POINT ( 'NONE',  ( 18.62500000000064659, -60.39062499999985079, -7.714727599197336083 ) ) ;
#5815 = B_SPLINE_CURVE_WITH_KNOTS ( 'NONE', 3,
 ( #9558, #11225, #14908, #10962 ),
 .UNSPECIFIED., .F., .F.,
 ( 4, 4 ),
 ( 2.383248697825728792E-07, 0.007646667935218603301 ),
 .UNSPECIFIED. ) ;
#5816 = CARTESIAN_POINT ( 'NONE',  ( 10.66717994462818453, 54.11542978231774725, 8.274144942030686067 ) ) ;
#5817 = CARTESIAN_POINT ( 'NONE',  ( -3.253207560246772267, 64.29697931017841483, -13.10216303624528678 ) ) ;
#5818 = ORIENTED_EDGE ( 'NONE', *, *, #2057, .T. ) ;
#5819 = CARTESIAN_POINT ( 'NONE',  ( -5.519522428242297885, 34.38017859743614935, -12.32010052773795117 ) ) ;
#5820 = CARTESIAN_POINT ( 'NONE',  ( -8.043339635997654113, -60.35624999999985363, 8.043339635996302306 ) ) ;
#5821 = CARTESIAN_POINT ( 'NONE',  ( 12.86350982126121423, 78.28284642631409440, 4.096370210139349766 ) ) ;
#5822 = CARTESIAN_POINT ( 'NONE',  ( -15.32135601632717403, 7.956016702382084915, 10.18318151426807816 ) ) ;
#5823 = EDGE_CURVE ( 'NONE', #10105, #13703, #200, .T. ) ;
#5824 = CARTESIAN_POINT ( 'NONE',  ( -2.138189944381240881, 37.60311857767972299, 13.49999999999999822 ) ) ;
#5825 = CARTESIAN_POINT ( 'NONE',  ( 12.98023825795362285, 72.56264182897429293, -3.709933363244806159 ) ) ;
#5826 = CARTESIAN_POINT ( 'NONE',  ( -4.171729424061787483, -12.66999999999999993, -12.83926296998457417 ) ) ;
#5827 = CIRCLE ( 'NONE', #8087, 3.624999999999999556 ) ;
#5828 = CARTESIAN_POINT ( 'NONE',  ( 4.171729424061789260, 65.82999999999999829, 12.83926296998457417 ) ) ;
#5829 = CARTESIAN_POINT ( 'NONE',  ( -13.20087293324353617, 53.02997338240815139, 2.826193941060762160 ) ) ;
#5830 = CARTESIAN_POINT ( 'NONE',  ( -9.520470885617717371, 36.22999999999999687, 6.917026985038133624 ) ) ;
#5831 = CARTESIAN_POINT ( 'NONE',  ( -8.343458848123582072, 55.37999999999998835, 11.48378591275254124 ) ) ;
#5832 = CARTESIAN_POINT ( 'NONE',  ( 2.894739436579920166E-06, 50.68008041434205069, 13.49999999999938005 ) ) ;
#5833 = CARTESIAN_POINT ( 'NONE',  ( 11.76794919243112680, -6.420000000000001705, -3.823638476888993942 ) ) ;
#5834 = CARTESIAN_POINT ( 'NONE',  ( 10.87711439316070994, 69.12741176127229892, 7.996158228696909731 ) ) ;
#5835 = CARTESIAN_POINT ( 'NONE',  ( 0.000000000000000000, -22.00000000000000000, 12.00000000000000178 ) ) ;
#5836 = CARTESIAN_POINT ( 'NONE',  ( -2.138189944381240881, 79.60311857767972299, 13.49999999999999822 ) ) ;
#5837 = CARTESIAN_POINT ( 'NONE',  ( 1.561832610794586740E-12, -94.66249999999980957, -18.62500000000000000 ) ) ;
#5838 = CARTESIAN_POINT ( 'NONE',  ( -13.30952709364465392, 73.85039203528728535, -2.265519377583317784 ) ) ;
#5839 = CIRCLE ( 'NONE', #752, 14.50000000000000000 ) ;
#5840 = CARTESIAN_POINT ( 'NONE',  ( -4.504434722200154617, 76.34205122430185497, -12.72642524997305280 ) ) ;
#5841 = LINE ( 'NONE', #1829, #826 ) ;
#5842 = DIRECTION ( 'NONE',  ( 0.8660254037844454800, 0.000000000000000000, -0.4999999999999881761 ) ) ;
#5843 = DIRECTION ( 'NONE',  ( 1.000000000000000000, 0.000000000000000000, 0.000000000000000000 ) ) ;
#5844 = CARTESIAN_POINT ( 'NONE',  ( -13.49999999999999822, 29.78000000000001180, -4.386415899144240349 ) ) ;
#5845 = CARTESIAN_POINT ( 'NONE',  ( -9.520470885617715595, -2.369999999999996998, -6.917026985038136289 ) ) ;
#5846 = CARTESIAN_POINT ( 'NONE',  ( 9.520470885617717371, 37.72999999999999687, -6.917026985038131848 ) ) ;
#5847 = CARTESIAN_POINT ( 'NONE',  ( 13.49999999999999822, -14.72000000000000242, 4.386415899144237684 ) ) ;
#5848 = EDGE_CURVE ( 'NONE', #11548, #6684, #10929, .T. ) ;
#5849 = CARTESIAN_POINT ( 'NONE',  ( -9.445309217286480319, 32.30909206433305769, 9.645539299803775890 ) ) ;
#5850 = CARTESIAN_POINT ( 'NONE',  ( 1.364733589292189020, 74.72907077985779267, 13.43087977156992707 ) ) ;
#5851 = CARTESIAN_POINT ( 'NONE',  ( 3.245949991204708063, 2.511656448626708457E-16, -15.01720290182594297 ) ) ;
#5852 = B_SPLINE_CURVE_WITH_KNOTS ( 'NONE', 3,
 ( #1622, #5534, #16288, #8544 ),
 .UNSPECIFIED., .F., .F.,
 ( 4, 4 ),
 ( 0.008723199174958463573, 0.01636875612029859914 ),
 .UNSPECIFIED. ) ;
#5853 = VECTOR ( 'NONE', #1530, 1000.000000000000000 ) ;
#5854 = DIRECTION ( 'NONE',  ( -1.000000000000000000, -1.734723475976807094E-16, -0.000000000000000000 ) ) ;
#5855 = CARTESIAN_POINT ( 'NONE',  ( -8.343458848123576743, 84.48000000000000398, -11.48378591275254301 ) ) ;
#5856 = CARTESIAN_POINT ( 'NONE',  ( 10.51668321839406950, 51.75308810284574434, -8.469583928564711428 ) ) ;
#5857 = CYLINDRICAL_SURFACE ( 'NONE', #6476, 9.000000000000000000 ) ;
#5858 = CARTESIAN_POINT ( 'NONE',  ( 7.592992521937700801, 36.89513823555898142, -11.16818768155278185 ) ) ;
#5859 = PLANE ( 'NONE',  #15581 ) ;
#5860 = DIRECTION ( 'NONE',  ( -0.000000000000000000, 1.000000000000000000, -0.000000000000000000 ) ) ;
#5861 = CARTESIAN_POINT ( 'NONE',  ( 6.020175498787003754, 62.89962116244318935, 12.09133458464389754 ) ) ;
#5862 = CARTESIAN_POINT ( 'NONE',  ( 13.49678185461208990, 42.41729046651699520, 0.3662733902496916882 ) ) ;
#5863 = CARTESIAN_POINT ( 'NONE',  ( 8.344294404855231662, 48.86157356941107821, -10.61324355268026842 ) ) ;
#5864 = CARTESIAN_POINT ( 'NONE',  ( -7.272992578804307939, 24.48000000000000398, -10.01041549318726886 ) ) ;
#5865 = ORIENTED_EDGE ( 'NONE', *, *, #9920, .T. ) ;
#5866 = CARTESIAN_POINT ( 'NONE',  ( 11.76794919243112325, 67.28000000000000114, 3.823638476888997051 ) ) ;
#5867 = CARTESIAN_POINT ( 'NONE',  ( -18.62500000000000000, -84.32499999999977547, -1.562973063126292757E-12 ) ) ;
#5868 = CARTESIAN_POINT ( 'NONE',  ( 4.711679271993006068, -46.82812499999987921, 11.37500000000039257 ) ) ;
#5869 = CARTESIAN_POINT ( 'NONE',  ( 10.92172942406179104, 3.730000000000011084, -7.935100905948385908 ) ) ;
#5870 = VERTEX_POINT ( 'NONE', #926 ) ;
#5871 = CARTESIAN_POINT ( 'NONE',  ( -0.4522785723817098757, 43.19626226204393760, -13.49242542680654644 ) ) ;
#5872 = DIRECTION ( 'NONE',  ( -0.000000000000000000, -1.000000000000000000, -0.000000000000000000 ) ) ;
#5873 = CARTESIAN_POINT ( 'NONE',  ( 10.92172942406178926, 1.129999999999992122, 7.935100905948385908 ) ) ;
#5874 = CARTESIAN_POINT ( 'NONE',  ( 7.714727599197339636, -13.52812499999996909, 18.62500000000063949 ) ) ;
#5875 = CARTESIAN_POINT ( 'NONE',  ( 12.19709600459181154, 66.21706713072794059, 5.804849116533907782 ) ) ;
#5876 = CARTESIAN_POINT ( 'NONE',  ( 1.488409699040705636, 56.73351772559257711, 13.41770261815923249 ) ) ;
#5877 = CARTESIAN_POINT ( 'NONE',  ( -7.272992578804307939, 62.47999999999998977, -10.01041549318726886 ) ) ;
#5878 = CARTESIAN_POINT ( 'NONE',  ( -10.92172942406179104, 34.22999999999999687, 7.935100905948387684 ) ) ;
#5879 = CARTESIAN_POINT ( 'NONE',  ( -3.636496289402153081, 71.32999999999999829, -11.19198476289190936 ) ) ;
#5880 = CARTESIAN_POINT ( 'NONE',  ( -13.29558833726832923, 46.84766757876133880, -2.340971711627301666 ) ) ;
#5881 = CARTESIAN_POINT ( 'NONE',  ( 9.154447501136807830, 45.82340124140479531, -9.922000396780600084 ) ) ;
#5882 = CARTESIAN_POINT ( 'NONE',  ( 5.635477359489657445, 69.97533625320679107, -12.26749346402417373 ) ) ;
#5883 = DIRECTION ( 'NONE',  ( -0.000000000000000000, 1.000000000000000000, -0.000000000000000000 ) ) ;
#5884 = CARTESIAN_POINT ( 'NONE',  ( 10.42314640861484065, 30.75812289050851689, -8.579516016103108100 ) ) ;
#5885 = CARTESIAN_POINT ( 'NONE',  ( -5.431336152102981707, 56.48321098987901223, 12.35944654956180777 ) ) ;
#5886 = CARTESIAN_POINT ( 'NONE',  ( 8.343458848123580296, 52.97999999999999687, 11.48378591275253768 ) ) ;
#5887 = CARTESIAN_POINT ( 'NONE',  ( 7.311496232511652593, 32.95290564063432726, 11.35083834095794408 ) ) ;
#5888 = B_SPLINE_CURVE_WITH_KNOTS ( 'NONE', 3,
 ( #10431, #1213, #14718, #10682 ),
 .UNSPECIFIED., .F., .F.,
 ( 4, 4 ),
 ( 2.383248697861188768E-07, 0.007646667935218598965 ),
 .UNSPECIFIED. ) ;
#5889 = CARTESIAN_POINT ( 'NONE',  ( -1.092208315176195654, 73.21924657073326159, -13.46228893901942669 ) ) ;
#5890 = CARTESIAN_POINT ( 'NONE',  ( 0.4650740877207917290, 40.16329413024163841, -13.49310518871272535 ) ) ;
#5891 = VERTEX_POINT ( 'NONE', #12954 ) ;
#5892 = CARTESIAN_POINT ( 'NONE',  ( -13.12312772325057431, 62.04431330923600996, 3.218249322805211587 ) ) ;
#5893 = CARTESIAN_POINT ( 'NONE',  ( -13.16986379959834252, -80.09374999999982947, -13.16986379960055409 ) ) ;
#5894 = CARTESIAN_POINT ( 'NONE',  ( 10.58196978195695515, 48.11063103762162285, 8.383901230509726688 ) ) ;
#5895 = CARTESIAN_POINT ( 'NONE',  ( 8.343458848123580296, 64.97999999999997556, 11.48378591275253768 ) ) ;
#5896 = CARTESIAN_POINT ( 'NONE',  ( 4.171729424061789260, 32.82999999999999829, 12.83926296998457417 ) ) ;
#5897 = CARTESIAN_POINT ( 'NONE',  ( -4.171729424061791036, 40.52999999999999403, 12.83926296998457239 ) ) ;
#5898 = CARTESIAN_POINT ( 'NONE',  ( -0.003427026735675507609, 46.18012310849080393, -13.50000000215092832 ) ) ;
#5899 = EDGE_CURVE ( 'NONE', #1880, #6127, #8733, .T. ) ;
#5900 = CARTESIAN_POINT ( 'NONE',  ( -10.55949117639465484, 67.60932008274608052, -8.413858223306061035 ) ) ;
#5901 = CARTESIAN_POINT ( 'NONE',  ( 18.62500000000000000, -42.69999999999988205, 1.560692158462880521E-12 ) ) ;
#5902 = CARTESIAN_POINT ( 'NONE',  ( 7.790142975789170698, 53.97365200280928121, 11.03460745363281426 ) ) ;
#5903 = ORIENTED_EDGE ( 'NONE', *, *, #7636, .F. ) ;
#5904 = CARTESIAN_POINT ( 'NONE',  ( -0.4727126854107578380, 64.19699700596120806, -13.49172460010241714 ) ) ;
#5905 = VERTEX_POINT ( 'NONE', #11723 ) ;
#5906 = CARTESIAN_POINT ( 'NONE',  ( 8.622924440245734345, 9.863741101803070066, -11.09913452436183867 ) ) ;
#5907 = CARTESIAN_POINT ( 'NONE',  ( -10.19441049769735130, 34.58951039502781555, -8.850085066458992955 ) ) ;
#5908 = CARTESIAN_POINT ( 'NONE',  ( 8.043339635996300530, -14.56874999999996589, 8.043339635997654113 ) ) ;
#5909 = AXIS2_PLACEMENT_3D ( 'NONE', #6271, #11917, #3782 ) ;
#5910 = CARTESIAN_POINT ( 'NONE',  ( 11.83416267854458326, 78.18933780232462993, 6.496366743272888655 ) ) ;
#5911 = CARTESIAN_POINT ( 'NONE',  ( -1.545162525932825686E-06, 79.18000005555833809, -13.49999999999990941 ) ) ;
#5912 = CARTESIAN_POINT ( 'NONE',  ( 7.500000000000001776, -27.73625732136942901, 2.063574628993722015 ) ) ;
#5913 = CARTESIAN_POINT ( 'NONE',  ( 13.04355863927429127, 72.55420972505207544, -3.483812310663820355 ) ) ;
#5914 = CARTESIAN_POINT ( 'NONE',  ( -9.520470885617715595, 33.62999999999999545, -6.917026985038136289 ) ) ;
#5915 = CARTESIAN_POINT ( 'NONE',  ( -8.343458848123576743, 67.48000000000000398, -11.48378591275254301 ) ) ;
#5916 = CARTESIAN_POINT ( 'NONE',  ( -1.929592546336893033, 52.24936810948035060, -13.36251507991583942 ) ) ;
#5917 = CARTESIAN_POINT ( 'NONE',  ( -11.76794919243112325, 38.92999999999999972, -2.882316262207890869E-15 ) ) ;
#5918 = CARTESIAN_POINT ( 'NONE',  ( -8.691771469529815392E-16, 61.67999999999999261, 14.19474002721660355 ) ) ;
#5919 = CARTESIAN_POINT ( 'NONE',  ( -15.34225977864763379, 8.027996330223285071, -9.656730951920845740 ) ) ;
#5920 = CARTESIAN_POINT ( 'NONE',  ( -3.636496289402152637, -2.669999999999998597, -11.19198476289190936 ) ) ;
#5921 = CARTESIAN_POINT ( 'NONE',  ( 7.621696303231366265, 68.96619805644265000, 11.14361944240803481 ) ) ;
#5922 = CARTESIAN_POINT ( 'NONE',  ( 5.883989548015875926, 30.92926152634062475, 10.19133431864935879 ) ) ;
#5923 = EDGE_CURVE ( 'NONE', #15045, #11619, #14348, .T. ) ;
#5924 = DIRECTION ( 'NONE',  ( 1.000000000000000000, 0.000000000000000000, 1.426480712616743416E-14 ) ) ;
#5925 = CARTESIAN_POINT ( 'NONE',  ( 7.714727599197340524, -104.0281249999997755, 18.62500000000063949 ) ) ;
#5926 = CARTESIAN_POINT ( 'NONE',  ( -13.42510730815057940, 73.98100147573404683, 1.466630498505447466 ) ) ;
#5927 = CARTESIAN_POINT ( 'NONE',  ( -2.715950498892019116, 76.27759078984141183, -13.22580361578473251 ) ) ;
#5928 = CARTESIAN_POINT ( 'NONE',  ( 0.000000000000000000, 3.000000000000000000, 0.000000000000000000 ) ) ;
#5929 = DIRECTION ( 'NONE',  ( -0.000000000000000000, -1.000000000000000000, -0.000000000000000000 ) ) ;
#5930 = CARTESIAN_POINT ( 'NONE',  ( 1.775737858763662015E-15, 9.999999999999998224, 14.50000000000000000 ) ) ;
#5931 = CARTESIAN_POINT ( 'NONE',  ( -9.520470885617715595, -5.370000000000000107, -6.917026985038136289 ) ) ;
#5932 = CARTESIAN_POINT ( 'NONE',  ( 9.520470885617715595, 40.12999999999999545, 6.917026985038134512 ) ) ;
#5933 = CARTESIAN_POINT ( 'NONE',  ( -10.92172942406178926, 1.629999999999992566, -7.935100905948389460 ) ) ;
#5934 = CARTESIAN_POINT ( 'NONE',  ( -11.28038879628374502, 32.20827684399202440, 7.416391123192743962 ) ) ;
#5935 = CYLINDRICAL_SURFACE ( 'NONE', #10232, 12.00000000000000178 ) ;
#5936 = VECTOR ( 'NONE', #15436, 1000.000000000000000 ) ;
#5937 = CARTESIAN_POINT ( 'NONE',  ( 4.171729424061791924, 4.030000000000005578, -12.83926296998457239 ) ) ;
#5938 = SHAPE_REPRESENTATION_RELATIONSHIP ( 'NONE' , 'NONE' ,  #5468, #1835 ) ;
#5939 = CARTESIAN_POINT ( 'NONE',  ( 2.272985001014427788E-15, 32.17999999999999972, -12.37355403259654985 ) ) ;
#5940 = CARTESIAN_POINT ( 'NONE',  ( 8.534827298566797893, 51.85287959032340410, -10.46283363410773681 ) ) ;
#5941 = LINE ( 'NONE', #2991, #17180 ) ;
#5942 = EDGE_CURVE ( 'NONE', #4960, #3997, #12337, .T. ) ;
#5943 = CARTESIAN_POINT ( 'NONE',  ( 1.653273178848926472E-15, 80.93000000000000682, 13.50000000000000000 ) ) ;
#5944 = DIRECTION ( 'NONE',  ( 1.000000000000000000, -0.000000000000000000, 9.821670480311996085E-15 ) ) ;
#5945 = DIRECTION ( 'NONE',  ( -0.000000000000000000, -1.000000000000000000, -0.000000000000000000 ) ) ;
#5946 = CARTESIAN_POINT ( 'NONE',  ( 10.64655758642687644, 63.11426932925019884, 8.300667950577015120 ) ) ;
#5947 = CARTESIAN_POINT ( 'NONE',  ( 0.5030752140698526720, 41.69808937357471024, 13.49082046348348385 ) ) ;
#5948 = CARTESIAN_POINT ( 'NONE',  ( 12.44133635878537625, 48.62102703855506292, -5.241715575524017012 ) ) ;
#5949 = CARTESIAN_POINT ( 'NONE',  ( -3.636496289402152637, 24.33000000000001961, -11.19198476289190936 ) ) ;
#5950 = ORIENTED_EDGE ( 'NONE', *, *, #6259, .T. ) ;
#5951 = CARTESIAN_POINT ( 'NONE',  ( 9.520470885617717371, 70.73000000000000398, -6.917026985038131848 ) ) ;
#5952 = CARTESIAN_POINT ( 'NONE',  ( -4.711679271993003404, 2.046875000000014211, -11.37500000000039613 ) ) ;
#5953 = CARTESIAN_POINT ( 'NONE',  ( -4.711679271993003404, -71.80312499999982379, -11.37500000000039435 ) ) ;
#5954 = CARTESIAN_POINT ( 'NONE',  ( -4.171729424061787483, 7.330000000000003624, -12.83926296998457417 ) ) ;
#5955 = EDGE_LOOP ( 'NONE', ( #8475, #1447, #12934, #12766 ) ) ;
#5956 = CARTESIAN_POINT ( 'NONE',  ( -9.520470885617715595, 33.62999999999999545, -6.917026985038136289 ) ) ;
#5957 = CARTESIAN_POINT ( 'NONE',  ( 1.668451422296728159, 80.92999999999999261, -13.07629037559559748 ) ) ;
#5958 = CARTESIAN_POINT ( 'NONE',  ( -10.92172942406178926, -0.3700000000000092104, -7.935100905948389460 ) ) ;
#5959 = CARTESIAN_POINT ( 'NONE',  ( 7.714727599200458030, -86.37187499999978968, -18.62499999999935341 ) ) ;
#5960 = CARTESIAN_POINT ( 'NONE',  ( 11.54972359916251889, 66.16909762691344099, 6.995529268059574868 ) ) ;
#5961 = CARTESIAN_POINT ( 'NONE',  ( 10.92172942406179104, 81.73000000000000398, -7.935100905948385908 ) ) ;
#5962 = CARTESIAN_POINT ( 'NONE',  ( 9.520470885617715595, 61.13000000000000256, 6.917026985038134512 ) ) ;
#5963 = CARTESIAN_POINT ( 'NONE',  ( -6.299567892059761753, 31.39042612893360484, 19.22554806868047805 ) ) ;
#5964 = CARTESIAN_POINT ( 'NONE',  ( 9.520470885617715595, 58.13000000000000256, 6.917026985038134512 ) ) ;
#5965 = CARTESIAN_POINT ( 'NONE',  ( -11.29930542946217109, 46.65291765115935618, -7.387593347751512773 ) ) ;
#5966 = CARTESIAN_POINT ( 'NONE',  ( 11.66267797177103738, 45.68289626953719562, -6.800399157363517411 ) ) ;
#5967 = CARTESIAN_POINT ( 'NONE',  ( 5.850572103796928047, 69.96703761332742033, -12.16734276622654320 ) ) ;
#5968 = CARTESIAN_POINT ( 'NONE',  ( -7.416407864998739718, 7.513974596215567736, 10.20780970022447853 ) ) ;
#5969 = CARTESIAN_POINT ( 'NONE',  ( 0.1944445437207606431, 31.17300849257853201, -13.49860884749332435 ) ) ;
#5970 = CARTESIAN_POINT ( 'NONE',  ( -13.45018538520116635, 55.97019992538123745, 1.159223571585510149 ) ) ;
#5971 = LINE ( 'NONE', #3298, #9241 ) ;
#5972 = CARTESIAN_POINT ( 'NONE',  ( 0.000000000000000000, 80.93000000000000682, 0.000000000000000000 ) ) ;
#5973 = CARTESIAN_POINT ( 'NONE',  ( 0.4129281128241998888, 43.16520274255920242, -13.49391189084656162 ) ) ;
#5974 = CARTESIAN_POINT ( 'NONE',  ( 12.14332122887934240, 39.64679378178001201, -5.899935319809511469 ) ) ;
#5975 = ORIENTED_EDGE ( 'NONE', *, *, #7675, .F. ) ;
#5976 = CARTESIAN_POINT ( 'NONE',  ( -11.08913010680831945, 62.22008114857175798, 7.699440692202677461 ) ) ;
#5977 = ORIENTED_EDGE ( 'NONE', *, *, #16517, .F. ) ;
#5978 = CARTESIAN_POINT ( 'NONE',  ( -13.08215237349078208, 40.81125640288357914, -3.336602680432516177 ) ) ;
#5979 = CARTESIAN_POINT ( 'NONE',  ( -8.343458848123576743, 34.48000000000000398, -11.48378591275254301 ) ) ;
#5980 = CARTESIAN_POINT ( 'NONE',  ( -13.16986379960055409, -84.25624999999983800, 13.16986379959834252 ) ) ;
#5981 = CARTESIAN_POINT ( 'NONE',  ( 13.06196386905416595, 48.30848771352356863, 3.411030766945946979 ) ) ;
#5982 = CARTESIAN_POINT ( 'NONE',  ( 4.478433445390353818, 58.01891974520321327, -12.73584891686745202 ) ) ;
#5983 = EDGE_CURVE ( 'NONE', #5515, #10469, #15351, .T. ) ;
#5984 = CARTESIAN_POINT ( 'NONE',  ( -13.50000000000000000, 37.92999999999999972, -3.306546357697853733E-15 ) ) ;
#5985 = CARTESIAN_POINT ( 'NONE',  ( 2.607531440858944223E-15, 39.17999999999999972, -14.19474002721660355 ) ) ;
#5986 = CARTESIAN_POINT ( 'NONE',  ( -7.576616670048093940E-16, 81.68000000000000682, 12.37355403259654985 ) ) ;
#5987 = CARTESIAN_POINT ( 'NONE',  ( 8.464728390624178894E-06, 46.17999963826949994, -13.49999999999734790 ) ) ;
#5988 = DIRECTION ( 'NONE',  ( -0.5000000000000006661, -0.000000000000000000, 0.8660254037844383745 ) ) ;
#5989 = CARTESIAN_POINT ( 'NONE',  ( -9.552639591052204498E-13, -5.237499999999969624, 11.37500000000000178 ) ) ;
#5990 = CARTESIAN_POINT ( 'NONE',  ( 4.344646002123737638, 53.83610922229849649, 12.78506762605347546 ) ) ;
#5991 = VERTEX_POINT ( 'NONE', #17211 ) ;
#5992 = CARTESIAN_POINT ( 'NONE',  ( -5.870390962563227788, 64.39383572203485073, -12.15683169922916917 ) ) ;
#5993 = ORIENTED_EDGE ( 'NONE', *, *, #12520, .T. ) ;
#5994 = VECTOR ( 'NONE', #14829, 1000.000000000000000 ) ;
#5995 = CARTESIAN_POINT ( 'NONE',  ( 4.743044421334680294, 67.00886042820928878, -12.64690991240490270 ) ) ;
#5996 = CARTESIAN_POINT ( 'NONE',  ( -5.508910881225164147, 34.37976951287060956, -12.32485102207323990 ) ) ;
#5997 = CARTESIAN_POINT ( 'NONE',  ( -8.043339635996302306, -72.84374999999981526, -8.043339635997654113 ) ) ;
#5998 = CARTESIAN_POINT ( 'NONE',  ( -17.14738331136000227, 7.815232041205461222, 7.999999999999841904 ) ) ;
#5999 = DIRECTION ( 'NONE',  ( 0.000000000000000000, 0.000000000000000000, 1.000000000000000000 ) ) ;
#6000 = CARTESIAN_POINT ( 'NONE',  ( 7.500000000000000000, -25.08364130939903092, 8.254396200996687583 ) ) ;
#6001 = CARTESIAN_POINT ( 'NONE',  ( 10.88156798610315512, 72.12748164754577829, 7.994026003792296109 ) ) ;
#6002 = CARTESIAN_POINT ( 'NONE',  ( 7.822218710939744746, 66.88499866975831765, -11.00287478893467785 ) ) ;
#6003 = CARTESIAN_POINT ( 'NONE',  ( 3.636496289402154414, 28.82999999999999474, 11.19198476289190758 ) ) ;
#6004 = CARTESIAN_POINT ( 'NONE',  ( -13.50000000000000000, 64.93000000000000682, -3.306546357697853733E-15 ) ) ;
#6005 = CARTESIAN_POINT ( 'NONE',  ( -9.135817427633982746, 52.53563195485393322, -9.940718253270615534 ) ) ;
#6006 = CARTESIAN_POINT ( 'NONE',  ( 7.272992578804311492, 37.87999999999999545, -10.01041549318726709 ) ) ;
#6007 = CARTESIAN_POINT ( 'NONE',  ( 11.76794919243112325, -15.71999999999999709, 3.823638476888996163 ) ) ;
#6008 = CARTESIAN_POINT ( 'NONE',  ( 13.50000000000000355, 56.57999999999999119, -4.386415899144233244 ) ) ;
#6009 = VECTOR ( 'NONE', #16103, 1000.000000000000000 ) ;
#6010 = DIRECTION ( 'NONE',  ( 0.000000000000000000, 0.000000000000000000, -1.000000000000000000 ) ) ;
#6011 = CARTESIAN_POINT ( 'NONE',  ( -11.76794919243112325, -2.220000000000004192, -3.823638476888998827 ) ) ;
#6012 = CARTESIAN_POINT ( 'NONE',  ( 9.918004550652394613, 69.07493629982988637, 9.158913472290203472 ) ) ;
#6013 = DIRECTION ( 'NONE',  ( 0.000000000000000000, -1.000000000000000000, 0.000000000000000000 ) ) ;
#6014 = CARTESIAN_POINT ( 'NONE',  ( 18.62500000000000000, 0.000000000000000000, 1.560692158462880521E-12 ) ) ;
#6015 = CARTESIAN_POINT ( 'NONE',  ( -12.64052664110000812, 73.75835914970723195, -4.739995431488866373 ) ) ;
#6016 = CARTESIAN_POINT ( 'NONE',  ( -5.827696143467630208, 76.39199596957689664, -12.18641047183595383 ) ) ;
#6017 = DIRECTION ( 'NONE',  ( 0.000000000000000000, -1.000000000000000000, 0.000000000000000000 ) ) ;
#6018 = CYLINDRICAL_SURFACE ( 'NONE', #14732, 12.00000000000000178 ) ;
#6019 = CARTESIAN_POINT ( 'NONE',  ( -3.636496289402152637, -5.669999999999994600, -11.19198476289190936 ) ) ;
#6020 = CARTESIAN_POINT ( 'NONE',  ( 3.636496289402154414, 36.82999999999999119, 11.19198476289190936 ) ) ;
#6021 = DIRECTION ( 'NONE',  ( 1.000000000000000000, 8.673617379884037937E-17, 0.000000000000000000 ) ) ;
#6022 = AXIS2_PLACEMENT_3D ( 'NONE', #1228, #15805, #3709 ) ;
#6023 = CARTESIAN_POINT ( 'NONE',  ( -4.024261390522248405, 32.53540582810948223, 12.88699713268044889 ) ) ;
#6024 = CARTESIAN_POINT ( 'NONE',  ( 1.523553703479234134, 74.73478094211517941, 13.41454831652031388 ) ) ;
#6025 = EDGE_CURVE ( 'NONE', #9365, #9130, #10254, .T. ) ;
#6026 = DIRECTION ( 'NONE',  ( -0.000000000000000000, -1.000000000000000000, -0.000000000000000000 ) ) ;
#6027 = CARTESIAN_POINT ( 'NONE',  ( 690.7486963872878505, 833.4303655526136936, 1297.674793841596738 ) ) ;
#6028 = CARTESIAN_POINT ( 'NONE',  ( 8.343458848123578520, 82.97999999999997556, 11.48378591275254124 ) ) ;
#6029 = CARTESIAN_POINT ( 'NONE',  ( 10.05803025841681198, 51.77773163741208151, -9.004780719399368749 ) ) ;
#6030 = CARTESIAN_POINT ( 'NONE',  ( 0.000000000000000000, 80.93000000000000682, -13.50000000000000000 ) ) ;
#6031 = AXIS2_PLACEMENT_3D ( 'NONE', #10238, #7410, #16931 ) ;
#6032 = CARTESIAN_POINT ( 'NONE',  ( 5.585016930642382249, 36.97714006553758281, -12.29076469185453746 ) ) ;
#6033 = CARTESIAN_POINT ( 'NONE',  ( 2.445080149700053643E-15, 75.17999999999999261, -13.50000000000000000 ) ) ;
#6034 = CARTESIAN_POINT ( 'NONE',  ( -2.115617638502927722, 49.25593553345355957, -13.34243514950316190 ) ) ;
#6035 = CARTESIAN_POINT ( 'NONE',  ( 9.872799149639176264, 63.07256805672663091, 9.208769869332330771 ) ) ;
#6036 = CARTESIAN_POINT ( 'NONE',  ( 0.8300164950611879089, 41.70984460997175347, 13.47471283487947069 ) ) ;
#6037 = CARTESIAN_POINT ( 'NONE',  ( 12.37575769567737538, 48.62700662711739596, -5.395588928150912622 ) ) ;
#6038 = CARTESIAN_POINT ( 'NONE',  ( -7.272992578804310604, 19.38000000000000256, 10.01041549318726709 ) ) ;
#6039 = ORIENTED_EDGE ( 'NONE', *, *, #2551, .T. ) ;
#6040 = CARTESIAN_POINT ( 'NONE',  ( -7.576616670048093940E-16, 66.67999999999999261, 12.37355403259654807 ) ) ;
#6041 = CARTESIAN_POINT ( 'NONE',  ( -11.37499999999960743, -33.33437499999990195, -4.711679271994912099 ) ) ;
#6042 = CARTESIAN_POINT ( 'NONE',  ( -11.37500000000000000, -41.62499999999990052, -9.545674412382054647E-13 ) ) ;
#6043 = CARTESIAN_POINT ( 'NONE',  ( 11.76794919243112325, 32.43000000000001393, 1.734723475976807094E-15 ) ) ;
#6044 = FACE_OUTER_BOUND ( 'NONE', #7103, .T. ) ;
#6045 =( BOUNDED_CURVE ( )  B_SPLINE_CURVE ( 2, ( #9092, #934, #6343, #14187, #17020, #3327, #2244, #6255, #7497, #11729, #5012, #766, #16846 ),
 .UNSPECIFIED., .F., .F. ) 
 B_SPLINE_CURVE_WITH_KNOTS ( ( 3, 2, 2, 2, 2, 2, 3 ),
 ( 0.4952864492504068794, 0.4981166612263263072, 0.5037770778311709829, 0.5094374944360154922, 0.5150979110408601125, 0.5207583276457047328, 0.5235885359481271539 ),
 .UNSPECIFIED. ) 
 CURVE ( )  GEOMETRIC_REPRESENTATION_ITEM ( )  RATIONAL_B_SPLINE_CURVE ( ( 0.9755282581476180104, 0.9755282263842351975, 1.000000000000000000, 0.9510565162951535312, 1.000000000000000000, 0.9510565162951535312, 1.000000000000000000, 0.9510565162951535312, 1.000000000000000000, 0.9510565162951535312, 1.000000000000000000, 0.9755282581475762660, 0.9755282581475768211 ) ) 
 REPRESENTATION_ITEM ( '' )  );
#6046 = ADVANCED_FACE ( 'NONE', ( #7780 ), #6361, .T. ) ;
#6047 = CARTESIAN_POINT ( 'NONE',  ( 7.714727599197339636, -30.17812499999993037, 18.62500000000063949 ) ) ;
#6048 = CARTESIAN_POINT ( 'NONE',  ( 5.773176358834770205, 65.89002590883258392, 12.20330810491806162 ) ) ;
#6049 = CARTESIAN_POINT ( 'NONE',  ( -10.92172942406179104, 80.22999999999998977, 7.935100905948387684 ) ) ;
#6050 = CARTESIAN_POINT ( 'NONE',  ( 11.76794919243112325, 46.27999999999999403, 3.823638476888996607 ) ) ;
#6051 = CARTESIAN_POINT ( 'NONE',  ( 9.335235950531815854E-15, 8.180000000000005045, -13.50000000000000178 ) ) ;
#6052 = CARTESIAN_POINT ( 'NONE',  ( -13.49064219070377746, 46.94729801505019395, 0.5027933102212878147 ) ) ;
#6053 = CARTESIAN_POINT ( 'NONE',  ( 9.420796519002903935, 45.81034643145268603, -9.670816597974919659 ) ) ;
#6054 = CARTESIAN_POINT ( 'NONE',  ( 8.045227603496410751, 69.87508753446272181, -10.84086963142225457 ) ) ;
#6055 = CARTESIAN_POINT ( 'NONE',  ( 10.43422754191850998, 30.75751561893000741, -8.566035940238601043 ) ) ;
#6056 = CARTESIAN_POINT ( 'NONE',  ( -11.06564900652519334, 56.22149449859761461, 7.733138918553730257 ) ) ;
#6057 = DIRECTION ( 'NONE',  ( 0.000000000000000000, 1.000000000000000000, 0.000000000000000000 ) ) ;
#6058 = CARTESIAN_POINT ( 'NONE',  ( 4.981677685877808237, 32.85966306824430916, 12.54919354416681188 ) ) ;
#6059 = CARTESIAN_POINT ( 'NONE',  ( 0.01063419157620585156, 43.17961891178009637, -13.49999685939349625 ) ) ;
#6060 = CARTESIAN_POINT ( 'NONE',  ( 12.46449749046236199, 39.61925870500666491, -5.200596085897637444 ) ) ;
#6061 = ORIENTED_EDGE ( 'NONE', *, *, #1742, .T. ) ;
#6062 = CARTESIAN_POINT ( 'NONE',  ( -12.71230713429092063, 62.09414301502697953, 4.544061370062732585 ) ) ;
#6063 = EDGE_LOOP ( 'NONE', ( #16401, #14674, #8822, #7557 ) ) ;
#6064 = EDGE_LOOP ( 'NONE', ( #17190, #12254, #15940, #7705 ) ) ;
#6065 = CARTESIAN_POINT ( 'NONE',  ( 0.1963306558083189324, -19.34015606061350923, 13.47512034797125580 ) ) ;
#6066 = CARTESIAN_POINT ( 'NONE',  ( -1.564113515457998370E-12, -102.9874999999997698, 18.62500000000000000 ) ) ;
#6067 = CARTESIAN_POINT ( 'NONE',  ( 11.74915954432862009, 48.18317559676947326, 6.649098532137857731 ) ) ;
#6068 = CARTESIAN_POINT ( 'NONE',  ( 9.335235950531815854E-15, 58.17999999999999972, -13.50000000000000178 ) ) ;
#6069 = CARTESIAN_POINT ( 'NONE',  ( 8.908714855037628055, 78.83534774718576443, -10.14565470230079391 ) ) ;
#6070 = B_SPLINE_CURVE_WITH_KNOTS ( 'NONE', 3,
 ( #17003, #10484, #10397, #3487, #5092, #13120, #7570, #14342, #2230, #15754, #2318, #3664, #1009, #9076, #7746, #15845, #3752, #14514, #17266, #5178, #10570, #15931, #2842, #8009, #215, #4188, #13546, #10913, #1265, #5269, #6677, #123, #5620, #9341, #1527, #1348, #12060, #7920, #13462, #16017, #6854, #16373, #17437, #8185, #13294, #17356, #8273, #2577, #12232, #13376, #10654, #5351, #6764, #5529, #16282, #10738, #13633, #11002, #16102, #1436, #9602, #12322 ),
 .UNSPECIFIED., .F., .F.,
 ( 4, 2, 2, 2, 2, 2, 2, 2, 2, 2, 2, 2, 2, 2, 2, 2, 2, 2, 2, 2, 2, 2, 2, 2, 2, 2, 2, 2, 2, 2, 4 ),
 ( 9.394995712984629401E-16, 0.002598098089080421499, 0.003897147133620162789, 0.005196196178159904512, 0.007794294267239384490, 0.009093343311779127081, 0.01039239235631886707, 0.01299049044539835052, 0.01428953948993809224, 0.01493906401220796570, 0.01558858853447783743, 0.01623811305674770916, 0.01656287531788264850, 0.01688763757901758783, 0.01721239984015252716, 0.01753716210128746650, 0.01818668662355734517, 0.01883621114582722383, 0.01948573566809710250, 0.02078478471263685290, 0.02208383375717660677, 0.02338288280171636063, 0.02468193184625611450, 0.02598098089079587183, 0.02857907897987538304, 0.03117717706895489424, 0.03377527515803439850, 0.03507432420257414890, 0.03637337324711390624, 0.03897147133619342091, 0.04156956942527292864 ),
 .UNSPECIFIED. ) ;
#6071 = CARTESIAN_POINT ( 'NONE',  ( -9.520470885617717371, 78.23000000000000398, 6.917026985038133624 ) ) ;
#6072 = CARTESIAN_POINT ( 'NONE',  ( 12.78300487269503805, -4.622062490413154417E-15, 1.228102481046923433 ) ) ;
#6073 = B_SPLINE_CURVE_WITH_KNOTS ( 'NONE', 3,
 ( #14560, #2274, #1052, #7875, #14385, #11759, #7963, #16061, #10695, #3796, #9208, #3969, #7794, #13252, #7700, #14301, #6464, #2443, #2188, #6375, #5045, #6285, #11673, #5223, #3706, #17048, #15802, #11849, #14473, #14647, #10609, #4954, #15976, #10357, #13333, #963, #15711, #9295, #1139, #3879, #10442, #9030, #9123, #1225, #11930, #12365, #12275, #2619, #1659, #6720, #8050, #13416, #8138, #8407, #9731, #10959, #2977, #14905, #14730, #9381, #16233, #6808, #15077, #11135, #7074, #172, #5577, #12458, #2799, #8319, #14815, #16508, #8230, #16327, #1306, #1393, #12186, #14995, #5751, #12098, #259, #78, #13503, #5483, #17480, #5667, #5394, #13591, #10779, #9467, #2887, #16143, #1485, #4142, #10865, #6902, #342, #4234, #4053, #2709, #13759, #9555, #9645, #13674, #1571, #6990, #11047, #16419, #4321, #3344, #5926, #8582, #8758, #8495, #4678, #11398, #6332, #6425, #14114, #7752, #15759, #691, #2000, #13933, #3669, #1014, #7243, #7426, #12806, #8669, #13125, #16770, #11809, #5004, #7334, #11721, #1827, #17096, #9997, #9082, #432, #5838, #12629, #10083, #10402, #3068, #15169, #13846, #6015, #14434, #1748, #9910, #7160, #2324, #4413, #9824, #15434, #12545, #11305, #11221, #16596, #4503, #15257, #16683, #3155, #517, #4590, #15345, #3246, #14026, #1915, #12718, #604, #17271, #14611, #5442, #1441, #14864, #8014, #13381, #2758, #2494, #13467, #10659, #6859, #9431, #16107, #1353, #17442, #5275, #1100, #5356, #2405, #4017, #7925, #15936, #13298, #14519, #8102, #3759, #3929, #2670, #17186, #10829, #3843, #8190, #12148, #14780, #6769, #9258, #13213, #1189, #37, #13552, #5185, #1271, #10743, #6600, #9171, #11980, #16191, #5097, #4103, #6515, #9519, #10489, #15851, #7840, #11896, #6683, #17361, #10575, #16022, #9346, #14695, #2582, #12065, #5889, #8629, #15041 ),
 .UNSPECIFIED., .F., .F.,
 ( 4, 2, 2, 2, 1, 1, 1, 2, 2, 2, 1, 1, 2, 2, 1, 1, 1, 1, 1, 2, 2, 1, 1, 2, 2, 1, 1, 2, 2, 1, 2, 2, 2, 2, 1, 1, 2, 2, 2, 2, 2, 1, 2, 2, 1, 1, 1, 1, 1, 2, 2, 1, 2, 2, 2, 2, 1, 1, 1, 2, 2, 2, 2, 1, 2, 2, 1, 1, 2, 2, 2, 2, 2, 2, 1, 1, 1, 1, 2, 2, 2, 2, 2, 1, 1, 1, 2, 2, 2, 2, 2, 2, 2, 2, 1, 1, 2, 2, 2, 1, 2, 2, 1, 1, 1, 2, 2, 1, 1, 2, 2, 2, 1, 2, 2, 1, 1, 2, 2, 2, 2, 1, 1, 2, 2, 1, 2, 2, 1, 2, 2, 1, 1, 2, 1, 2, 2, 1, 1, 2, 2, 2, 2, 2, 1, 1, 1, 2, 2, 4 ),
 ( 0.1227481640271067542, 0.1229765385430084124, 0.1229908119502522712, 0.1229979486538742006, 0.1230050853574961162, 0.1230336321719838338, 0.1230907258009592414, 0.1232049130589100705, 0.1236616620907133590, 0.1245751601543199499, 0.1248035346702215942, 0.1249177219281724233, 0.1249748155571478309, 0.1250033623716355347, 0.1250319091861232523, 0.1254886582179265131, 0.1259454072497297739, 0.1261737817656314320, 0.1262879690235822472, 0.1262951057272041766, 0.1263022424308260783, 0.1263165158380699371, 0.1263450626525576548, 0.1264021562815330901, 0.1268589053133364897, 0.1269159989423118973, 0.1269445457567996149, 0.1269516824604215444, 0.1269588191640434738, 0.1269730925712873326, 0.1270872798292382033, 0.1273156543451399447, 0.1282291524087469103, 0.1286859014405503931, 0.1288000886985012639, 0.1288571823274766992, 0.1288857291419644169, 0.1289142759564521346, 0.1291426504723538760, 0.1300561485359607583, 0.1305128975677642134, 0.1307412720836659270, 0.1308554593416167977, 0.1308840061561045154, 0.1309125529705922053, 0.1309696465995676407, 0.1314263956313710402, 0.1316547701472727538, 0.1317689574052236245, 0.1318260510341990321, 0.1318403244414428910, 0.1318545978486867498, 0.1318831446631744675, 0.1327966427267815441, 0.1328109161340254030, 0.1328180528376473324, 0.1328251895412692618, 0.1328537363557569795, 0.1329108299847323593, 0.1330250172426831745, 0.1332533917585847771, 0.1337101407903879824, 0.1346236388539943929, 0.1347378261119452081, 0.1347520995191890392, 0.1347663729264328980, 0.1347949197409206157, 0.1348520133698959955, 0.1350803878857975981, 0.1355371369176008312, 0.1364506349812072417, 0.1366790094971088443, 0.1367075563115965620, 0.1367361031260842519, 0.1367931967550596595, 0.1369073840130104469, 0.1373641330448136522, 0.1375925075607152270, 0.1376496011896906346, 0.1377066948186660422, 0.1378208820766168297, 0.1382776311084200072, 0.1385060056243216098, 0.1386201928822723972, 0.1386487396967600871, 0.1386630131040039460, 0.1386701498076258754, 0.1386772865112477771, 0.1387343801402231847, 0.1391911291720262234, 0.1401046272356323008, 0.1405613762674353395, 0.1406184698964107194, 0.1406470167108984093, 0.1406755635253860992, 0.1407897507833368866, 0.1410181252992384060, 0.1419316233628445389, 0.1423883723946476054, 0.1425025596525983651, 0.1425596532815737449, 0.1425882000960614349, 0.1426167469105491248, 0.1428451214264506719, 0.1433018704582537661, 0.1435302449741553132, 0.1435587917886430032, 0.1435873386031306931, 0.1436444322321060729, 0.1437586194900568604, 0.1442153685218600101, 0.1444437430377615850, 0.1445008366667369648, 0.1445293834812246825, 0.1445365201848465841, 0.1445436568884685136, 0.1445579302957123446, 0.1446721175536630488, 0.1455856156172688487, 0.1460423646490717209, 0.1462707391649731847, 0.1463849264229238889, 0.1464420200518992687, 0.1464705668663869309, 0.1464848402736307897, 0.1464991136808746208, 0.1474126117444803652, 0.1483261098080860818, 0.1483832034370614339, 0.1484117502515491238, 0.1484402970660367860, 0.1485544843239875179, 0.1487828588398889540, 0.1492396078716918262, 0.1493537951296425303, 0.1494108887586178824, 0.1494251621658617413, 0.1494394355731055724, 0.1494679823875932623, 0.1496963569034947261, 0.1501531059352976538, 0.1503814804511991177, 0.1503886171548210471, 0.1503957538584429765, 0.1504100272656868076, 0.1504385740801744975, 0.1504956677091498496, 0.1506098549671005815, 0.1510666039989035092, 0.1519801020625093646 ),
 .UNSPECIFIED. ) ;
#6074 = AXIS2_PLACEMENT_3D ( 'NONE', #3957, #159, #8039 ) ;
#6075 = CARTESIAN_POINT ( 'NONE',  ( -0.06432022310792409603, 46.18231244616364251, -13.49986851205962424 ) ) ;
#6076 = CARTESIAN_POINT ( 'NONE',  ( -0.1337557719945228207, 67.18480936409068249, -13.49933757132007628 ) ) ;
#6077 = CARTESIAN_POINT ( 'NONE',  ( -11.37500000000039790, -35.41562499999989200, 4.711679271993001628 ) ) ;
#6078 = CARTESIAN_POINT ( 'NONE',  ( 6.644535271319878866, 53.92494203076220316, 11.75165990948425154 ) ) ;
#6079 = ADVANCED_FACE ( 'NONE', ( #17122 ), #6460, .T. ) ;
#6080 = B_SPLINE_CURVE_WITH_KNOTS ( 'NONE', 3,
 ( #2002, #779, #10251, #3430 ),
 .UNSPECIFIED., .F., .F.,
 ( 4, 4 ),
 ( 2.376698214958262694E-07, 0.007646667280170314253 ),
 .UNSPECIFIED. ) ;
#6081 = ORIENTED_EDGE ( 'NONE', *, *, #15210, .F. ) ;
#6082 = PLANE ( 'NONE',  #10093 ) ;
#6083 = ORIENTED_EDGE ( 'NONE', *, *, #17408, .T. ) ;
#6084 = CARTESIAN_POINT ( 'NONE',  ( 13.49999999999999822, 9.280000000000002913, 4.386415899144236796 ) ) ;
#6085 = CARTESIAN_POINT ( 'NONE',  ( -4.731689125201891777, 34.35038980843969370, -12.64542749166197844 ) ) ;
#6086 = CARTESIAN_POINT ( 'NONE',  ( -11.37500000000000000, -91.57499999999977547, -9.545674412382054647E-13 ) ) ;
#6087 = CARTESIAN_POINT ( 'NONE',  ( 3.101660632740125934, 77.79147361761071977, 13.14641033372065415 ) ) ;
#6088 = CARTESIAN_POINT ( 'NONE',  ( 1.653273178848926472E-15, 0.000000000000000000, 13.50000000000000000 ) ) ;
#6089 = CARTESIAN_POINT ( 'NONE',  ( 15.78643792884164299, 8.055054264001460851, 8.704847339800551254 ) ) ;
#6090 = DIRECTION ( 'NONE',  ( 0.000000000000000000, 1.000000000000000000, 0.000000000000000000 ) ) ;
#6091 = CARTESIAN_POINT ( 'NONE',  ( 13.49760795208683284, 72.41181223906431796, 0.5098544550378681928 ) ) ;
#6092 = CARTESIAN_POINT ( 'NONE',  ( -11.76794919243112325, 31.07999999999999829, 3.823638476888994386 ) ) ;
#6093 = CARTESIAN_POINT ( 'NONE',  ( 10.92172942406179104, 63.72999999999999687, -7.935100905948385908 ) ) ;
#6094 = CARTESIAN_POINT ( 'NONE',  ( -0.3351920408089422709, 71.66794772448770345, 13.49586090856208820 ) ) ;
#6095 = CARTESIAN_POINT ( 'NONE',  ( -9.520470885617715595, 38.62999999999999545, -6.917026985038136289 ) ) ;
#6096 = CARTESIAN_POINT ( 'NONE',  ( 7.272992578804308828, -16.02000000000000313, 10.01041549318726709 ) ) ;
#6097 = CARTESIAN_POINT ( 'NONE',  ( -8.343458848123576743, 57.48000000000000398, -11.48378591275254301 ) ) ;
#6098 = CARTESIAN_POINT ( 'NONE',  ( 18.71385749420391420, 7.854010659623985369, -1.541332980592505120 ) ) ;
#6099 = CARTESIAN_POINT ( 'NONE',  ( -9.520470885617715595, 0.6299999999999916778, -6.917026985038136289 ) ) ;
#6100 = CARTESIAN_POINT ( 'NONE',  ( 3.426020828344902736, 68.80323833450283644, 13.05809747433249868 ) ) ;
#6101 = CARTESIAN_POINT ( 'NONE',  ( -1.564113515457998572E-12, -45.78749999999988773, 18.62500000000000000 ) ) ;
#6102 = CARTESIAN_POINT ( 'NONE',  ( -19.29752010712864418, 0.000000000000000000, 17.42428528562836831 ) ) ;
#6103 = CARTESIAN_POINT ( 'NONE',  ( -18.62500000000064659, -42.66562499999989200, 7.714727599197335195 ) ) ;
#6104 = CARTESIAN_POINT ( 'NONE',  ( -2.381931281991595206, 65.59435760367297519, 13.28825607429043387 ) ) ;
#6105 = CARTESIAN_POINT ( 'NONE',  ( 0.000000000000000000, 9.000000000000000000, 0.000000000000000000 ) ) ;
#6106 = CARTESIAN_POINT ( 'NONE',  ( -13.50000000000000000, 2.930000000000001936, -3.469446951953614189E-15 ) ) ;
#6107 = ORIENTED_EDGE ( 'NONE', *, *, #15386, .F. ) ;
#6108 = CARTESIAN_POINT ( 'NONE',  ( -9.520470885617715595, 41.63000000000000256, -6.917026985038136289 ) ) ;
#6109 = AXIS2_PLACEMENT_3D ( 'NONE', #3158, #12548, #4326 ) ;
#6110 = CARTESIAN_POINT ( 'NONE',  ( 10.92172942406178926, 80.13000000000000966, 7.935100905948387684 ) ) ;
#6111 = CARTESIAN_POINT ( 'NONE',  ( -13.39519961485953026, 31.86913630564962929, -1.748191886245508364 ) ) ;
#6112 = CARTESIAN_POINT ( 'NONE',  ( 2.042046933105797546, 74.75341727322346230, 13.34690593482024212 ) ) ;
#6113 = CARTESIAN_POINT ( 'NONE',  ( 2.755455298081545172E-15, 3.000000000000000000, 22.50000000000000355 ) ) ;
#6114 = CARTESIAN_POINT ( 'NONE',  ( -10.92172942406178926, 78.63000000000000966, -7.935100905948389460 ) ) ;
#6115 = CARTESIAN_POINT ( 'NONE',  ( 12.65245305301080414, 51.60041585730986213, -4.708045043639258687 ) ) ;
#6116 = AXIS2_PLACEMENT_3D ( 'NONE', #1241, #8071, #14834 ) ;
#6117 = CARTESIAN_POINT ( 'NONE',  ( -11.21035395369201915, 38.21266103485134380, 7.521839952431427889 ) ) ;
#6118 = CARTESIAN_POINT ( 'NONE',  ( 10.32492466292448974, 36.76347586491808528, -8.697596036060231128 ) ) ;
#6119 = CARTESIAN_POINT ( 'NONE',  ( -8.043339635996300530, -13.49374999999998614, -8.043339635997652337 ) ) ;
#6120 = EDGE_CURVE ( 'NONE', #16109, #6426, #6916, .T. ) ;
#6121 = DIRECTION ( 'NONE',  ( -0.000000000000000000, -1.000000000000000000, -0.000000000000000000 ) ) ;
#6122 = CARTESIAN_POINT ( 'NONE',  ( 1.653273178848926472E-15, 80.93000000000000682, 13.50000000000000000 ) ) ;
#6123 = CARTESIAN_POINT ( 'NONE',  ( -2.419409634026826961, 80.59289594391761113, 13.28325634299493707 ) ) ;
#6124 = CARTESIAN_POINT ( 'NONE',  ( 4.457234882645010110, 41.84008533871757152, 12.75041784350807106 ) ) ;
#6125 = CARTESIAN_POINT ( 'NONE',  ( 13.49762871381596874, 48.42116860337419126, 0.2575671418023918746 ) ) ;
#6126 = CARTESIAN_POINT ( 'NONE',  ( 7.272992578804311492, 14.88000000000000078, -10.01041549318726709 ) ) ;
#6127 = VERTEX_POINT ( 'NONE', #14289 ) ;
#6128 = CARTESIAN_POINT ( 'NONE',  ( 7.272992578804308828, 69.97999999999998977, 10.01041549318726886 ) ) ;
#6129 = CARTESIAN_POINT ( 'NONE',  ( 13.16986379960055409, -78.08124999999978400, -13.16986379959834430 ) ) ;
#6130 = CARTESIAN_POINT ( 'NONE',  ( 8.343458848123580296, 55.97999999999999687, 11.48378591275253768 ) ) ;
#6131 = CARTESIAN_POINT ( 'NONE',  ( -11.76794919243112325, 31.07999999999999829, 3.823638476888994386 ) ) ;
#6132 = CARTESIAN_POINT ( 'NONE',  ( 1.133384680211434459, 76.13924943277646662, -13.45318893631145052 ) ) ;
#6133 = CIRCLE ( 'NONE', #5561, 6.000000000000000000 ) ;
#6134 = CARTESIAN_POINT ( 'NONE',  ( -7.714727599200466912, -78.04687499999982947, 18.62499999999934985 ) ) ;
#6135 = CARTESIAN_POINT ( 'NONE',  ( 10.16039061381173525, 66.08774085974377499, 8.889160252383520699 ) ) ;
#6136 = CARTESIAN_POINT ( 'NONE',  ( 10.92172942406179104, 78.72999999999998977, -7.935100905948385908 ) ) ;
#6137 = CARTESIAN_POINT ( 'NONE',  ( -3.636496289402153081, 53.33000000000000540, -11.19198476289190936 ) ) ;
#6138 = CARTESIAN_POINT ( 'NONE',  ( 13.50000000000000355, 7.580000000000000071, -4.386415899144233244 ) ) ;
#6139 = CARTESIAN_POINT ( 'NONE',  ( -9.938087151227913196, 59.28401552682182540, 9.136990211801220951 ) ) ;
#6140 = CARTESIAN_POINT ( 'NONE',  ( 13.16726819044754393, 45.53581346377539063, -2.986114351398691191 ) ) ;
#6141 = CARTESIAN_POINT ( 'NONE',  ( 10.14020416995585983, 69.77338333202821730, -8.912142960987960549 ) ) ;
#6142 = SURFACE_STYLE_USAGE ( .BOTH. , #3307 ) ;
#6143 = CARTESIAN_POINT ( 'NONE',  ( 13.23463183243080366, 30.52433186400915588, -2.671914872127473473 ) ) ;
#6144 = CARTESIAN_POINT ( 'NONE',  ( -13.47837838110856090, 55.90363568160458385, -0.7637818885891087817 ) ) ;
#6145 = ADVANCED_FACE ( 'NONE', ( #2087 ), #9195, .T. ) ;
#6146 = FACE_OUTER_BOUND ( 'NONE', #1355, .T. ) ;
#6147 = PLANE ( 'NONE',  #5088 ) ;
#6148 = CARTESIAN_POINT ( 'NONE',  ( 2.755455298081545172E-15, 3.000000000000000000, 22.50000000000000355 ) ) ;
#6149 = CARTESIAN_POINT ( 'NONE',  ( 12.95691110344991337, 39.56579465547967089, -3.794630013198587282 ) ) ;
#6150 = ORIENTED_EDGE ( 'NONE', *, *, #5216, .F. ) ;
#6151 = CARTESIAN_POINT ( 'NONE',  ( 7.329991333342587900, -1.736202706843529944E-17, -9.501117147637041072 ) ) ;
#6152 = CARTESIAN_POINT ( 'NONE',  ( -12.99103486005599883, 61.79864889427442876, -3.678670038247435325 ) ) ;
#6153 = ORIENTED_EDGE ( 'NONE', *, *, #14837, .T. ) ;
#6154 = ORIENTED_EDGE ( 'NONE', *, *, #1901, .F. ) ;
#6155 = CARTESIAN_POINT ( 'NONE',  ( 4.171729424061791924, 31.03000000000000114, -12.83926296998457239 ) ) ;
#6156 = CARTESIAN_POINT ( 'NONE',  ( -13.16986379960055231, -27.05624999999993463, 13.16986379959834252 ) ) ;
#6157 = CARTESIAN_POINT ( 'NONE',  ( 6.919944324611998709, 57.92390741887160743, -11.60445687867207987 ) ) ;
#6158 = CARTESIAN_POINT ( 'NONE',  ( 10.71171996125772985, 78.74211244272670740, -8.219364172421744996 ) ) ;
#6159 = CARTESIAN_POINT ( 'NONE',  ( 9.520470885617717371, 82.73000000000000398, -6.917026985038131848 ) ) ;
#6160 = CARTESIAN_POINT ( 'NONE',  ( -13.49999999999999822, 43.07999999999999829, 4.386415899144235908 ) ) ;
#6161 = CARTESIAN_POINT ( 'NONE',  ( -11.76794919243112325, 83.78000000000001535, -3.823638476888998827 ) ) ;
#6162 = DIRECTION ( 'NONE',  ( 0.000000000000000000, -1.000000000000000000, 0.000000000000000000 ) ) ;
#6163 = CARTESIAN_POINT ( 'NONE',  ( -4.711679271994916540, -20.84687499999993321, 11.37499999999960565 ) ) ;
#6164 = ADVANCED_FACE ( 'NONE', ( #6537 ), #9013, .T. ) ;
#6165 = CARTESIAN_POINT ( 'NONE',  ( 9.453713556340927582, 54.05132085550528842, 9.637327269826936771 ) ) ;
#6166 = ORIENTED_EDGE ( 'NONE', *, *, #11694, .T. ) ;
#6167 = PLANE ( 'NONE',  #4427 ) ;
#6168 = VERTEX_POINT ( 'NONE', #14460 ) ;
#6169 = CARTESIAN_POINT ( 'NONE',  ( 1.408343819019457359E-15, 0.000000000000000000, -9.500000000000021316 ) ) ;
#6170 = CARTESIAN_POINT ( 'NONE',  ( -8.043339635997652337, -17.65624999999997513, 8.043339635996300530 ) ) ;
#6171 = LINE ( 'NONE', #3497, #8627 ) ;
#6172 = CARTESIAN_POINT ( 'NONE',  ( -3.851070442117878745, 59.54153006582451013, 12.93912176508445810 ) ) ;
#6173 = PLANE ( 'NONE',  #17372 ) ;
#6174 = DIRECTION ( 'NONE',  ( 0.000000000000000000, 0.000000000000000000, 1.000000000000000000 ) ) ;
#6175 = CARTESIAN_POINT ( 'NONE',  ( 12.68447996868631122, 72.26291114008931515, 4.621164343339557057 ) ) ;
#6176 = CARTESIAN_POINT ( 'NONE',  ( 11.76794919243112680, 29.58000000000000540, -3.823638476888993942 ) ) ;
#6177 = CARTESIAN_POINT ( 'NONE',  ( 8.343458848123583849, 48.87999999999998835, -11.48378591275253768 ) ) ;
#6178 = CARTESIAN_POINT ( 'NONE',  ( -0.3911409227513171771, 71.66593604615781032, 13.49433737296981306 ) ) ;
#6179 = DIRECTION ( 'NONE',  ( 0.000000000000000000, -1.000000000000000000, 0.000000000000000000 ) ) ;
#6180 = CARTESIAN_POINT ( 'NONE',  ( -4.282754437214131293, 68.52600206748782341, 12.80272888647489893 ) ) ;
#6181 = CARTESIAN_POINT ( 'NONE',  ( -18.62500000000000000, -58.27499999999986358, -1.562973063126292555E-12 ) ) ;
#6182 = CARTESIAN_POINT ( 'NONE',  ( 18.62362042714189059, -100.0000000000000000, 0.000000000000000000 ) ) ;
#6183 = AXIS2_PLACEMENT_3D ( 'NONE', #17465, #9281, #4129 ) ;
#6184 = CARTESIAN_POINT ( 'NONE',  ( -13.16986379959834252, -6.243749999999985256, -13.16986379960055054 ) ) ;
#6185 = CARTESIAN_POINT ( 'NONE',  ( -5.734174865113238262, 65.47163811465718197, 12.22337932611075573 ) ) ;
#6186 = CARTESIAN_POINT ( 'NONE',  ( -11.80445978200331503, 80.92999999999996419, -1.125850548943733376 ) ) ;
#6187 = DIRECTION ( 'NONE',  ( 0.000000000000000000, -1.000000000000000000, 0.000000000000000000 ) ) ;
#6188 = EDGE_LOOP ( 'NONE', ( #12241, #322, #3577, #10512, #6468, #14051, #15323, #3739, #15224, #2406, #9060, #3694, #8715, #3005, #11916, #10446, #3304, #9350 ) ) ;
#6189 = CARTESIAN_POINT ( 'NONE',  ( -3.636496289402153081, 32.32999999999999829, -11.19198476289190936 ) ) ;
#6190 = CARTESIAN_POINT ( 'NONE',  ( -2.883235578040820091, 40.28367049126757138, -13.18852187992278502 ) ) ;
#6191 = CARTESIAN_POINT ( 'NONE',  ( -12.52052419915814063, 31.74586622497447408, -5.068148337449895457 ) ) ;
#6192 = CARTESIAN_POINT ( 'NONE',  ( 8.148423059287221548, 74.98954435357713066, 10.76380695295465273 ) ) ;
#6193 = CARTESIAN_POINT ( 'NONE',  ( 11.56270653563395356, 60.17021069121303611, 6.968727811706270536 ) ) ;
#6194 = CARTESIAN_POINT ( 'NONE',  ( 8.343458848123583849, 62.88000000000000256, -11.48378591275253768 ) ) ;
#6195 = CIRCLE ( 'NONE', #7608, 12.00000000000000178 ) ;
#6196 = EDGE_CURVE ( 'NONE', #7733, #7293, #3171, .T. ) ;
#6197 = CARTESIAN_POINT ( 'NONE',  ( 11.32976262874806395, 51.70524724435282593, -7.343873846068756706 ) ) ;
#6198 = CARTESIAN_POINT ( 'NONE',  ( -12.55208093682576909, 38.11047456955122925, 4.969580869381986510 ) ) ;
#6199 = CARTESIAN_POINT ( 'NONE',  ( 12.20992711788400520, 36.64133221546218522, -5.762380518153004338 ) ) ;
#6200 = CARTESIAN_POINT ( 'NONE',  ( -4.711679271993001628, -62.40312499999986073, -11.37500000000039613 ) ) ;
#6201 = CARTESIAN_POINT ( 'NONE',  ( 24.73863375370598305, 0.000000000000000000, -7.999999999999934275 ) ) ;
#6202 = CARTESIAN_POINT ( 'NONE',  ( -3.800243545151680280, 77.54335724604808888, 12.95408144013974194 ) ) ;
#6203 = LINE ( 'NONE', #11589, #16638 ) ;
#6204 = CARTESIAN_POINT ( 'NONE',  ( -7.499999999999998224, 108.9300000000000068, 9.367496997597600128 ) ) ;
#6205 = CARTESIAN_POINT ( 'NONE',  ( 13.47608760677475459, 48.40154206234144851, 0.8241170574654087533 ) ) ;
#6206 = CARTESIAN_POINT ( 'NONE',  ( -11.76794919243112325, 15.92999999999999972, -2.602085213965210642E-15 ) ) ;
#6207 = ORIENTED_EDGE ( 'NONE', *, *, #14312, .F. ) ;
#6208 = CARTESIAN_POINT ( 'NONE',  ( -3.636496289402155746, 60.53000000000000114, 11.19198476289190936 ) ) ;
#6209 = CARTESIAN_POINT ( 'NONE',  ( 8.043339635997652337, -28.13124999999991260, -8.043339635996304082 ) ) ;
#6210 = CARTESIAN_POINT ( 'NONE',  ( -11.37500000000039613, -92.61562499999978115, 4.711679271993001628 ) ) ;
#6211 = CARTESIAN_POINT ( 'NONE',  ( 2.621994543952811015E-15, -1.820000000000002283, -14.19474002721660355 ) ) ;
#6212 = CARTESIAN_POINT ( 'NONE',  ( 11.76794919243112325, 29.43000000000001037, 1.734723475976807094E-15 ) ) ;
#6213 = DIRECTION ( 'NONE',  ( 0.000000000000000000, 0.000000000000000000, -1.000000000000000000 ) ) ;
#6214 = CARTESIAN_POINT ( 'NONE',  ( -7.714727599200466912, -44.74687499999989626, 18.62499999999934985 ) ) ;
#6215 = CARTESIAN_POINT ( 'NONE',  ( 2.607531440858944223E-15, 82.18000000000000682, -14.19474002721660355 ) ) ;
#6216 = EDGE_CURVE ( 'NONE', #11530, #13318, #6705, .T. ) ;
#6217 = CARTESIAN_POINT ( 'NONE',  ( -11.76794919243112325, 48.07999999999998408, 3.823638476888994386 ) ) ;
#6218 = DIRECTION ( 'NONE',  ( -0.000000000000000000, -1.000000000000000000, -0.000000000000000000 ) ) ;
#6219 = CARTESIAN_POINT ( 'NONE',  ( -13.47905022307413603, 58.90402517245511405, -0.7520165846117183861 ) ) ;
#6220 = CARTESIAN_POINT ( 'NONE',  ( 11.55642355312311942, 45.16972346798684868, 6.979809178588280538 ) ) ;
#6221 = DIRECTION ( 'NONE',  ( 0.000000000000000000, -1.000000000000000000, 0.000000000000000000 ) ) ;
#6222 = CARTESIAN_POINT ( 'NONE',  ( 1.529356327037144636, 80.73498994847588506, 13.41315609044504065 ) ) ;
#6223 = CARTESIAN_POINT ( 'NONE',  ( 12.02353733592099161, 30.65632963770153196, -6.138774346578745877 ) ) ;
#6224 = CARTESIAN_POINT ( 'NONE',  ( -13.28969977581182071, 55.84641863258806893, -2.375863902518644988 ) ) ;
#6225 = CARTESIAN_POINT ( 'NONE',  ( -13.42114948243943218, 49.98161693057358690, 1.483081436913393780 ) ) ;
#6226 = CARTESIAN_POINT ( 'NONE',  ( 3.017866001013571609, 64.07148374553901249, -13.15915560476493162 ) ) ;
#6227 = DIRECTION ( 'NONE',  ( -0.8660254037844365982, 0.000000000000000000, -0.5000000000000035527 ) ) ;
#6228 = CARTESIAN_POINT ( 'NONE',  ( 13.09506756767692082, 39.54674493898122734, -3.282300712200310944 ) ) ;
#6229 = ORIENTED_EDGE ( 'NONE', *, *, #9898, .T. ) ;
#6230 = CARTESIAN_POINT ( 'NONE',  ( -7.131439210029803633, 61.44517228716789248, -11.46358492120966766 ) ) ;
#6231 = VERTEX_POINT ( 'NONE', #8035 ) ;
#6232 = EDGE_LOOP ( 'NONE', ( #9106, #11703, #6929, #5336 ) ) ;
#6233 = CARTESIAN_POINT ( 'NONE',  ( -4.171729424061791036, 32.53000000000000114, 12.83926296998457239 ) ) ;
#6234 = CARTESIAN_POINT ( 'NONE',  ( -13.16986379959834252, -39.54374999999990337, -13.16986379960055054 ) ) ;
#6235 = CARTESIAN_POINT ( 'NONE',  ( 13.06645423851852073, 48.30912723757910499, 3.393787163694668152 ) ) ;
#6236 = LINE ( 'NONE', #16739, #12442 ) ;
#6237 = CARTESIAN_POINT ( 'NONE',  ( 0.5008926393039752067, 79.16199793852693745, -13.49195660129378460 ) ) ;
#6238 = CARTESIAN_POINT ( 'NONE',  ( -3.636496289402155746, 75.53000000000000114, 11.19198476289190936 ) ) ;
#6239 = CARTESIAN_POINT ( 'NONE',  ( 4.171729424061791924, 39.03000000000000114, -12.83926296998457239 ) ) ;
#6240 = CARTESIAN_POINT ( 'NONE',  ( 10.85239523646640336, -2.258074356960818337E-15, 7.640122180002231644 ) ) ;
#6241 = ADVANCED_FACE ( 'NONE', ( #6973 ), #2604, .T. ) ;
#6242 = CARTESIAN_POINT ( 'NONE',  ( 1.732050807568877415, 7.773118517290098950, -19.00000000000000000 ) ) ;
#6243 = CARTESIAN_POINT ( 'NONE',  ( -0.1463139935563050886, 67.18526091003258216, -13.49920831200174831 ) ) ;
#6244 = CARTESIAN_POINT ( 'NONE',  ( -11.37500000000039790, -52.06562499999986926, 4.711679271993001628 ) ) ;
#6245 = CARTESIAN_POINT ( 'NONE',  ( -4.171729424061787483, 78.32999999999999829, -12.83926296998457417 ) ) ;
#6246 = CARTESIAN_POINT ( 'NONE',  ( 5.770345405016722218, 33.97008500761054250, -12.20464375447771488 ) ) ;
#6247 = ORIENTED_EDGE ( 'NONE', *, *, #1763, .T. ) ;
#6248 = CARTESIAN_POINT ( 'NONE',  ( 8.377273874081270222, 10.00009955288323127, 10.58637257760431361 ) ) ;
#6249 = EDGE_LOOP ( 'NONE', ( #1964, #5950 ) ) ;
#6250 = CARTESIAN_POINT ( 'NONE',  ( 2.372771011195240920, 67.09468957437705683, -13.29338533608859585 ) ) ;
#6251 = CARTESIAN_POINT ( 'NONE',  ( 8.043339635997652337, -42.63124999999990905, -8.043339635996302306 ) ) ;
#6252 = CARTESIAN_POINT ( 'NONE',  ( 4.338753566204257339, 77.83602819694414165, 12.78390686162523338 ) ) ;
#6253 = CARTESIAN_POINT ( 'NONE',  ( -0.3413906785081720074, 59.66772483089536649, 13.49568742704858160 ) ) ;
#6254 = FACE_OUTER_BOUND ( 'NONE', #4740, .T. ) ;
#6255 = CARTESIAN_POINT ( 'NONE',  ( -13.49999999999999822, 5.779999999999997584, -4.386415899144240349 ) ) ;
#6256 = CARTESIAN_POINT ( 'NONE',  ( 0.7476565982748099026, 71.70685699333597540, 13.50000000000422951 ) ) ;
#6257 = CARTESIAN_POINT ( 'NONE',  ( 13.49999999999999822, 51.27999999999998693, 4.386415899144237684 ) ) ;
#6258 = CARTESIAN_POINT ( 'NONE',  ( -5.788310938635475189, 71.46938236682071022, 12.19612480893602147 ) ) ;
#6259 = EDGE_CURVE ( 'NONE', #5187, #12977, #14887, .T. ) ;
#6260 = CARTESIAN_POINT ( 'NONE',  ( 18.85009555739749487, 7.815224737767794139, -1.645503437279525416 ) ) ;
#6261 = CARTESIAN_POINT ( 'NONE',  ( -7.714727599197335195, -71.80312499999982379, -18.62500000000064304 ) ) ;
#6262 = CARTESIAN_POINT ( 'NONE',  ( -4.406206840049315510, 68.52151906854182073, 12.76072571588954929 ) ) ;
#6263 = CARTESIAN_POINT ( 'NONE',  ( 13.16986379959834075, -31.21874999999992539, 13.16986379960055231 ) ) ;
#6264 = CARTESIAN_POINT ( 'NONE',  ( 2.909063323423874969, 55.07541729461457436, -13.18314304101936507 ) ) ;
#6265 = CARTESIAN_POINT ( 'NONE',  ( -7.714727599200467800, -28.09687499999992966, 18.62499999999934630 ) ) ;
#6266 = CARTESIAN_POINT ( 'NONE',  ( -9.403854346568712330, 65.31129198192570584, 9.690887349900259906 ) ) ;
#6267 = CARTESIAN_POINT ( 'NONE',  ( 3.708203932499368527, 7.696025403784440222, 11.41267819554184371 ) ) ;
#6268 = CARTESIAN_POINT ( 'NONE',  ( -11.24427269215573588, 35.21054676296952124, 7.471034886962134358 ) ) ;
#6269 = CARTESIAN_POINT ( 'NONE',  ( -10.92172942406179104, 27.23000000000000398, 7.935100905948385908 ) ) ;
#6270 = ORIENTED_EDGE ( 'NONE', *, *, #3966, .T. ) ;
#6271 = CARTESIAN_POINT ( 'NONE',  ( 0.000000000000000000, 0.000000000000000000, 0.000000000000000000 ) ) ;
#6272 = CARTESIAN_POINT ( 'NONE',  ( -4.492754712431366038, 40.34163550128833009, -12.73059084564603971 ) ) ;
#6273 = CARTESIAN_POINT ( 'NONE',  ( -13.43211739905840751, 31.88231842745090105, -1.376614423219626238 ) ) ;
#6274 = DIRECTION ( 'NONE',  ( 0.000000000000000000, 1.000000000000000000, 0.000000000000000000 ) ) ;
#6275 = CARTESIAN_POINT ( 'NONE',  ( 10.82852970008509708, 60.12463039269763954, 8.062284012199853578 ) ) ;
#6276 = CARTESIAN_POINT ( 'NONE',  ( 8.343458848123583849, -1.120000000000002327, -11.48378591275253768 ) ) ;
#6277 = CARTESIAN_POINT ( 'NONE',  ( 4.171729424061789260, 2.829999999999999183, 12.83926296998457239 ) ) ;
#6278 = VECTOR ( 'NONE', #15613, 1000.000000000000000 ) ;
#6279 = CARTESIAN_POINT ( 'NONE',  ( -9.520470885617715595, 59.63000000000000256, -6.917026985038136289 ) ) ;
#6280 = CARTESIAN_POINT ( 'NONE',  ( 13.50000000000000355, 74.58000000000001251, -4.386415899144233244 ) ) ;
#6281 = CARTESIAN_POINT ( 'NONE',  ( 12.96113944439583143, 51.56544759790433119, -3.784739602708540041 ) ) ;
#6282 = CARTESIAN_POINT ( 'NONE',  ( -13.33882841394733987, 38.00291347817611154, 2.079824949345720597 ) ) ;
#6283 = CARTESIAN_POINT ( 'NONE',  ( 13.35680911868298892, 36.50067082660722662, -2.019122932424611605 ) ) ;
#6284 = CARTESIAN_POINT ( 'NONE',  ( -8.043339635996300530, -63.44374999999985931, -8.043339635997652337 ) ) ;
#6285 = CARTESIAN_POINT ( 'NONE',  ( -3.467007694106094107, 74.55533922032466876, 13.04722352598931145 ) ) ;
#6286 = CARTESIAN_POINT ( 'NONE',  ( -11.20645768432849998, 77.21280782326037695, 7.531521138223463474 ) ) ;
#6287 = AXIS2_PLACEMENT_3D ( 'NONE', #6511, #8097, #17182 ) ;
#6288 = CARTESIAN_POINT ( 'NONE',  ( 0.3932787996077972692, 62.69414064364450923, 13.49440792938528588 ) ) ;
#6289 = CARTESIAN_POINT ( 'NONE',  ( 2.314350980473266706, 41.76329157920511648, 13.31043818058748585 ) ) ;
#6290 = ORIENTED_EDGE ( 'NONE', *, *, #14194, .T. ) ;
#6291 = CARTESIAN_POINT ( 'NONE',  ( 2.279995255611139653E-15, 15.18000000000000504, -12.37355403259654985 ) ) ;
#6292 = EDGE_CURVE ( 'NONE', #9130, #13814, #5298, .T. ) ;
#6293 = EDGE_LOOP ( 'NONE', ( #9587, #10061, #16731, #5903 ) ) ;
#6294 = CARTESIAN_POINT ( 'NONE',  ( 3.636496289402157078, 59.03000000000000114, -11.19198476289190936 ) ) ;
#6295 = CARTESIAN_POINT ( 'NONE',  ( -4.711679271994916540, -54.14687499999985931, 11.37499999999960565 ) ) ;
#6296 = CARTESIAN_POINT ( 'NONE',  ( 10.92172942406178926, 56.13000000000000256, 7.935100905948387684 ) ) ;
#6297 = CARTESIAN_POINT ( 'NONE',  ( -8.549982208541774191E-16, -3.319999999999998064, 14.19474002721660355 ) ) ;
#6298 = CARTESIAN_POINT ( 'NONE',  ( 3.647687574545794842, 76.04884256590771940, -12.99786464873113800 ) ) ;
#6299 = CARTESIAN_POINT ( 'NONE',  ( 13.16986379959834075, -64.51874999999984084, 13.16986379960055231 ) ) ;
#6300 = DIRECTION ( 'NONE',  ( -0.000000000000000000, 1.000000000000000000, -0.000000000000000000 ) ) ;
#6301 = CARTESIAN_POINT ( 'NONE',  ( 3.636496289402154414, 48.82999999999999829, 11.19198476289190936 ) ) ;
#6302 = PLANE ( 'NONE',  #10340 ) ;
#6303 = AXIS2_PLACEMENT_3D ( 'NONE', #12932, #2127, #8970 ) ;
#6304 = CARTESIAN_POINT ( 'NONE',  ( -13.00542838102342103, 59.05976455672130498, 3.627390584878091406 ) ) ;
#6305 = CARTESIAN_POINT ( 'NONE',  ( 13.02807058628658154, 45.30366086987346819, 3.541023234573203560 ) ) ;
#6306 = CARTESIAN_POINT ( 'NONE',  ( 13.40107646287879106, 69.37314970047374629, 1.632315145005664769 ) ) ;
#6307 = DIRECTION ( 'NONE',  ( -0.8660254037844326014, 0.000000000000000000, -0.5000000000000104361 ) ) ;
#6308 = CARTESIAN_POINT ( 'NONE',  ( 13.49017281487221709, 30.44772149245933335, -0.5150320868971011157 ) ) ;
#6309 = CARTESIAN_POINT ( 'NONE',  ( -11.05190432090530095, 56.22231890020226075, 7.752779392575588346 ) ) ;
#6310 = CARTESIAN_POINT ( 'NONE',  ( -8.000342243122073427, 50.37758064104690447, 10.89743709494727675 ) ) ;
#6311 = CYLINDRICAL_SURFACE ( 'NONE', #14927, 13.50000000000000000 ) ;
#6312 = CARTESIAN_POINT ( 'NONE',  ( 3.419293449951197772, 43.05708390336630487, -13.06129965743578225 ) ) ;
#6313 = CARTESIAN_POINT ( 'NONE',  ( 7.866618816620490229, 38.97691562748362770, 10.98017853868179827 ) ) ;
#6314 = ORIENTED_EDGE ( 'NONE', *, *, #15264, .F. ) ;
#6315 = CARTESIAN_POINT ( 'NONE',  ( -4.064505406101394769, 61.32614459997894585, -12.87361187749841207 ) ) ;
#6316 = CARTESIAN_POINT ( 'NONE',  ( 11.76794919243112325, 5.279999999999999361, 3.823638476888996163 ) ) ;
#6317 = ORIENTED_EDGE ( 'NONE', *, *, #11024, .F. ) ;
#6318 = CARTESIAN_POINT ( 'NONE',  ( -11.90455661557854405, 40.69456295689673908, -6.366441307886505641 ) ) ;
#6319 = EDGE_LOOP ( 'NONE', ( #4376, #2449 ) ) ;
#6320 = CARTESIAN_POINT ( 'NONE',  ( 11.76794919243112325, -18.56999999999999673, 1.734723475976807094E-15 ) ) ;
#6321 = CARTESIAN_POINT ( 'NONE',  ( 18.62500000000064304, -1.040624999999997469, -7.714727599197335195 ) ) ;
#6322 = CARTESIAN_POINT ( 'NONE',  ( 6.632571939248276927, 47.92442758682717141, 11.75836653333053938 ) ) ;
#6323 = CARTESIAN_POINT ( 'NONE',  ( 11.55679130585532377, 57.69021217686731973, -6.977864065983907516 ) ) ;
#6324 = CARTESIAN_POINT ( 'NONE',  ( 9.155849417392163403, 78.82336870447842614, -9.921330499117095414 ) ) ;
#6325 = CARTESIAN_POINT ( 'NONE',  ( 11.76794919243112680, 79.57999999999999829, -3.823638476888993942 ) ) ;
#6326 = CARTESIAN_POINT ( 'NONE',  ( 7.272992578804311492, 82.87999999999999545, -10.01041549318726709 ) ) ;
#6327 = CYLINDRICAL_SURFACE ( 'NONE', #10151, 12.00000000000000178 ) ;
#6328 = LINE ( 'NONE', #7397, #15570 ) ;
#6329 = CARTESIAN_POINT ( 'NONE',  ( 4.711679271994911211, -62.47187499999984084, -11.37499999999960743 ) ) ;
#6330 = CARTESIAN_POINT ( 'NONE',  ( -7.500000000000000000, 98.93000000000002103, 1.224646799147353059E-15 ) ) ;
#6331 = CARTESIAN_POINT ( 'NONE',  ( 5.783632216765496104, 33.96956555804999311, -12.19835297658227979 ) ) ;
#6332 = CARTESIAN_POINT ( 'NONE',  ( -13.47745682340583606, 73.95692245389201958, 0.7799622905020241470 ) ) ;
#6333 = ADVANCED_FACE ( 'NONE', ( #8123 ), #7947, .T. ) ;
#6334 = EDGE_LOOP ( 'NONE', ( #10128, #12609 ) ) ;
#6335 = DIRECTION ( 'NONE',  ( 0.000000000000000000, -1.000000000000000000, 0.000000000000000000 ) ) ;
#6336 = EDGE_CURVE ( 'NONE', #14477, #14459, #14705, .T. ) ;
#6337 = ORIENTED_EDGE ( 'NONE', *, *, #16969, .F. ) ;
#6338 = CARTESIAN_POINT ( 'NONE',  ( 8.343458848123583849, 15.87999999999999901, -11.48378591275253768 ) ) ;
#6339 = CARTESIAN_POINT ( 'NONE',  ( 8.043339635997652337, -25.98124999999995310, -8.043339635996302306 ) ) ;
#6340 = DIRECTION ( 'NONE',  ( -0.000000000000000000, 1.000000000000000000, -0.000000000000000000 ) ) ;
#6341 = CARTESIAN_POINT ( 'NONE',  ( -7.201777607271541370, 59.41183315282604838, 11.41860466315153388 ) ) ;
#6342 = CARTESIAN_POINT ( 'NONE',  ( 7.500000000000000000, 108.9300000000000068, -12.00000000000000178 ) ) ;
#6343 = CARTESIAN_POINT ( 'NONE',  ( -4.171729424061791036, 6.530000000000008242, 12.83926296998457239 ) ) ;
#6344 = CARTESIAN_POINT ( 'NONE',  ( -10.92172942406179104, 53.22999999999999687, 7.935100905948387684 ) ) ;
#6345 = CARTESIAN_POINT ( 'NONE',  ( 13.49999999999999822, 50.27999999999999403, 4.386415899144237684 ) ) ;
#6346 = CARTESIAN_POINT ( 'NONE',  ( -3.158365208622146092, 71.56643682723847633, 13.12534696263546685 ) ) ;
#6347 =( BOUNDED_CURVE ( )  B_SPLINE_CURVE ( 2, ( #6423, #7923, #8012, #3757, #9256, #15757, #17440, #15849, #6513, #3575, #14345, #11894, #2234 ),
 .UNSPECIFIED., .F., .F. ) 
 B_SPLINE_CURVE_WITH_KNOTS ( ( 3, 2, 2, 2, 2, 2, 3 ),
 ( 0.7361111111111110494, 0.7388888888888889284, 0.7444444444444444642, 0.7500000000000000000, 0.7555555555555555358, 0.7611111111111110716, 0.7638888888888888395 ),
 .UNSPECIFIED. ) 
 CURVE ( )  GEOMETRIC_REPRESENTATION_ITEM ( )  RATIONAL_B_SPLINE_CURVE ( ( 0.9755282581475768211, 0.9755282581475762660, 1.000000000000000000, 0.9510565162951535312, 1.000000000000000000, 0.9510565162951535312, 1.000000000000000000, 0.9510565162951535312, 1.000000000000000000, 0.9510565162951535312, 1.000000000000000000, 0.9755282581475772652, 0.9755282581475768211 ) ) 
 REPRESENTATION_ITEM ( '' )  );
#6348 = CARTESIAN_POINT ( 'NONE',  ( 20.00000000000000000, 0.000000000000000000, 7.056441485635107799E-14 ) ) ;
#6349 = CARTESIAN_POINT ( 'NONE',  ( 18.62499999999934630, -82.20937499999980957, 7.714727599200467800 ) ) ;
#6350 = CARTESIAN_POINT ( 'NONE',  ( 1.608760344010755849, 68.73785721169490159, 13.40460866987880451 ) ) ;
#6351 = CARTESIAN_POINT ( 'NONE',  ( 13.16986379960055054, -52.03124999999987921, -13.16986379959834430 ) ) ;
#6352 = CARTESIAN_POINT ( 'NONE',  ( 15.58845726811984811, 7.773118517290097174, 11.00000000000007283 ) ) ;
#6353 = CARTESIAN_POINT ( 'NONE',  ( 13.16986379960055054, -18.73124999999995666, -13.16986379959834430 ) ) ;
#6354 = CARTESIAN_POINT ( 'NONE',  ( -7.494032182223336669, 65.39933563442717457, 11.22954942317015181 ) ) ;
#6355 = EDGE_CURVE ( 'NONE', #4352, #11548, #2682, .T. ) ;
#6356 = DIRECTION ( 'NONE',  ( 0.000000000000000000, -1.000000000000000000, 0.000000000000000000 ) ) ;
#6357 = AXIS2_PLACEMENT_3D ( 'NONE', #14371, #6021, #699 ) ;
#6358 = CARTESIAN_POINT ( 'NONE',  ( -1.627500644183926592, 35.62147431220920168, 13.40154254870227035 ) ) ;
#6359 = CARTESIAN_POINT ( 'NONE',  ( 2.621994543952811015E-15, 23.17999999999999616, -14.19474002721660355 ) ) ;
#6360 = VERTEX_POINT ( 'NONE', #10944 ) ;
#6361 = CYLINDRICAL_SURFACE ( 'NONE', #8165, 22.50000000000000355 ) ;
#6362 = DIRECTION ( 'NONE',  ( -0.000000000000000000, -1.000000000000000000, -0.000000000000000000 ) ) ;
#6363 = CARTESIAN_POINT ( 'NONE',  ( 8.343458848123580296, 79.98000000000000398, 11.48378591275253768 ) ) ;
#6364 = CARTESIAN_POINT ( 'NONE',  ( -12.95925257371713890, 32.06574706565864830, 3.792278602194695036 ) ) ;
#6365 = DIRECTION ( 'NONE',  ( -0.000000000000000000, -1.000000000000000000, -0.000000000000000000 ) ) ;
#6366 = CARTESIAN_POINT ( 'NONE',  ( 10.77435480767992004, 60.12150780088424540, 8.134627539065268920 ) ) ;
#6367 = CARTESIAN_POINT ( 'NONE',  ( 13.50000000000000000, -4.569999999999997620, 1.734723475976807094E-15 ) ) ;
#6368 = CARTESIAN_POINT ( 'NONE',  ( -11.94568210041848211, 53.16233194022309050, 6.289003155707704629 ) ) ;
#6369 = CARTESIAN_POINT ( 'NONE',  ( -3.636496289402153081, 56.32999999999999829, -11.19198476289190936 ) ) ;
#6370 = CONTEXT_DEPENDENT_SHAPE_REPRESENTATION ( #12295, #8051 ) ;
#6371 = CARTESIAN_POINT ( 'NONE',  ( 11.59569013348710165, 51.68756802306698006, -6.913263822545960835 ) ) ;
#6372 = CARTESIAN_POINT ( 'NONE',  ( -10.49833770927574328, 38.25438360216252676, 8.492147799501781336 ) ) ;
#6373 = CARTESIAN_POINT ( 'NONE',  ( 10.14797380081446931, 36.77298809516717881, -8.903775999886867965 ) ) ;
#6374 = CARTESIAN_POINT ( 'NONE',  ( 11.37500000000039613, -74.89062499999985789, -4.711679271993002516 ) ) ;
#6375 = CARTESIAN_POINT ( 'NONE',  ( -3.427855787583714786, 74.55674710714738751, 13.05757467429366336 ) ) ;
#6376 = VECTOR ( 'NONE', #7404, 1000.000000000000000 ) ;
#6377 = CARTESIAN_POINT ( 'NONE',  ( -9.860018955205955393, 77.28819560419356094, 9.231716877605229854 ) ) ;
#6378 = EDGE_CURVE ( 'NONE', #5891, #2325, #16310, .T. ) ;
#6379 = CARTESIAN_POINT ( 'NONE',  ( -4.171729424061791036, 61.53000000000000114, 12.83926296998457239 ) ) ;
#6380 = LINE ( 'NONE', #11763, #3464 ) ;
#6381 = VERTEX_POINT ( 'NONE', #12351 ) ;
#6382 = CARTESIAN_POINT ( 'NONE',  ( -9.520470885617715595, 9.629999999999999005, -6.917026985038136289 ) ) ;
#6383 = VERTEX_POINT ( 'NONE', #5650 ) ;
#6384 = CARTESIAN_POINT ( 'NONE',  ( 11.76794919243112680, 55.58000000000000540, -3.823638476888993942 ) ) ;
#6385 = CARTESIAN_POINT ( 'NONE',  ( -9.552639591052204498E-13, -38.53749999999988063, 11.37500000000000178 ) ) ;
#6386 = DIRECTION ( 'NONE',  ( 0.000000000000000000, 0.000000000000000000, -1.000000000000000000 ) ) ;
#6387 = CARTESIAN_POINT ( 'NONE',  ( 10.64789061155650884, 75.74566424434127043, -8.299534072142243701 ) ) ;
#6388 = CARTESIAN_POINT ( 'NONE',  ( 7.272992578804308828, 33.97999999999999687, 10.01041549318726709 ) ) ;
#6389 = DIRECTION ( 'NONE',  ( 0.000000000000000000, -1.000000000000000000, 0.000000000000000000 ) ) ;
#6390 = CARTESIAN_POINT ( 'NONE',  ( -10.92172942406179104, 68.23000000000000398, 7.935100905948387684 ) ) ;
#6391 = CIRCLE ( 'NONE', #14274, 12.00000000000000178 ) ;
#6392 = CARTESIAN_POINT ( 'NONE',  ( -9.520470885617715595, 53.62999999999999545, -6.917026985038136289 ) ) ;
#6393 = DIRECTION ( 'NONE',  ( -0.5000056658327881598, 0.000000000000000000, -0.8660221325896412248 ) ) ;
#6394 = CARTESIAN_POINT ( 'NONE',  ( -9.891505788093740037, 59.28644356468626597, 9.187487902970126186 ) ) ;
#6395 = CARTESIAN_POINT ( 'NONE',  ( 12.08007619667642629, 45.20759642052237837, 6.045378948472979630 ) ) ;
#6396 = CARTESIAN_POINT ( 'NONE',  ( 11.92386745150823835, 69.66398541232135244, -6.330266153154159525 ) ) ;
#6397 = FACE_OUTER_BOUND ( 'NONE', #14504, .T. ) ;
#6398 = CARTESIAN_POINT ( 'NONE',  ( 12.98311147291790668, 30.29531732055727034, 3.773380263830190096 ) ) ;
#6399 = CARTESIAN_POINT ( 'NONE',  ( -4.385685656986241909, 55.33775113349322083, -12.76810838760984979 ) ) ;
#6400 = CARTESIAN_POINT ( 'NONE',  ( -13.45332018961691567, 49.96890492016202501, 1.122494546679217997 ) ) ;
#6401 = CARTESIAN_POINT ( 'NONE',  ( 19.29752010712851984, 5.918584287042171432, -17.42428528562851042 ) ) ;
#6402 = CARTESIAN_POINT ( 'NONE',  ( 5.641315611847744549, 42.97511016371111481, -12.26481840930462930 ) ) ;
#6403 = CARTESIAN_POINT ( 'NONE',  ( 13.32130220385322517, 39.35314012507830483, 2.189450966719809433 ) ) ;
#6404 = ORIENTED_EDGE ( 'NONE', *, *, #10040, .F. ) ;
#6405 = CARTESIAN_POINT ( 'NONE',  ( -6.536041484435296312, 70.42036142381789432, -11.81975216884413626 ) ) ;
#6406 = CARTESIAN_POINT ( 'NONE',  ( -9.590357845055994090, 61.55798154981976467, -9.505963504770354788 ) ) ;
#6407 = VECTOR ( 'NONE', #3267, 1000.000000000000000 ) ;
#6408 = CARTESIAN_POINT ( 'NONE',  ( 3.636496289402154414, 1.829999999999998295, 11.19198476289190758 ) ) ;
#6409 = ORIENTED_EDGE ( 'NONE', *, *, #5455, .F. ) ;
#6410 = CARTESIAN_POINT ( 'NONE',  ( -8.149994195541450992, 40.48961995060131613, -10.76232869325634667 ) ) ;
#6411 = ORIENTED_EDGE ( 'NONE', *, *, #9029, .T. ) ;
#6412 = CARTESIAN_POINT ( 'NONE',  ( 10.92172942406179104, 24.73000000000000043, -7.935100905948385908 ) ) ;
#6413 = CARTESIAN_POINT ( 'NONE',  ( -18.62499999999934985, -90.53437499999978400, -7.714727599200458918 ) ) ;
#6414 = CARTESIAN_POINT ( 'NONE',  ( 13.39116189056811734, 57.37028256231064205, 1.710872541480398468 ) ) ;
#6415 = CARTESIAN_POINT ( 'NONE',  ( 12.23576758771793749, 78.63913862522007037, -5.705453660566566221 ) ) ;
#6416 = CARTESIAN_POINT ( 'NONE',  ( 3.636496289402157078, 80.03000000000000114, -11.19198476289190936 ) ) ;
#6417 = CARTESIAN_POINT ( 'NONE',  ( -9.520470885617717371, 75.23000000000000398, 6.917026985038133624 ) ) ;
#6418 = DIRECTION ( 'NONE',  ( 0.000000000000000000, 0.000000000000000000, -1.000000000000000000 ) ) ;
#6419 = AXIS2_PLACEMENT_3D ( 'NONE', #17359, #10657, #14432 ) ;
#6420 =( NAMED_UNIT ( * ) SI_UNIT ( $, .STERADIAN. ) SOLID_ANGLE_UNIT ( ) );
#6421 = DIRECTION ( 'NONE',  ( 1.000000000000000000, 0.000000000000000000, -0.000000000000000000 ) ) ;
#6422 = CARTESIAN_POINT ( 'NONE',  ( 8.043339635997652337, -78.08124999999978400, -8.043339635996304082 ) ) ;
#6423 = CARTESIAN_POINT ( 'NONE',  ( -8.291044507619272909E-14, 45.17999999999999972, -13.50000000000000000 ) ) ;
#6424 = CARTESIAN_POINT ( 'NONE',  ( 10.21170435963994549, 33.76958486911632207, -8.830561736147624075 ) ) ;
#6425 = CARTESIAN_POINT ( 'NONE',  ( -13.47976463482231857, 73.95550874856458279, 0.7393779786335853421 ) ) ;
#6426 = VERTEX_POINT ( 'NONE', #3865 ) ;
#6427 = VERTEX_POINT ( 'NONE', #12441 ) ;
#6428 = DIRECTION ( 'NONE',  ( -1.301042606982605567E-16, 1.000000000000000000, 0.000000000000000000 ) ) ;
#6429 = ORIENTED_EDGE ( 'NONE', *, *, #1152, .T. ) ;
#6430 = CARTESIAN_POINT ( 'NONE',  ( -4.171729424061787483, 13.33000000000000895, -12.83926296998457417 ) ) ;
#6431 = CARTESIAN_POINT ( 'NONE',  ( 3.636496289402157078, -11.96999999999999531, -11.19198476289190936 ) ) ;
#6432 = CARTESIAN_POINT ( 'NONE',  ( 11.37499999999999645, -23.89999999999996305, 9.531744055041752924E-13 ) ) ;
#6433 = DIRECTION ( 'NONE',  ( -0.000000000000000000, 1.000000000000000000, -0.000000000000000000 ) ) ;
#6434 = FACE_OUTER_BOUND ( 'NONE', #7056, .T. ) ;
#6435 = CARTESIAN_POINT ( 'NONE',  ( 9.880245923157088939, 66.78702064977453290, -9.199584342333487541 ) ) ;
#6436 = CARTESIAN_POINT ( 'NONE',  ( -8.343458848123582072, 50.37999999999999545, 11.48378591275254124 ) ) ;
#6437 = CARTESIAN_POINT ( 'NONE',  ( -11.74928976714265261, 71.17669313983024892, 6.649811694681813989 ) ) ;
#6438 = EDGE_CURVE ( 'NONE', #16836, #14499, #10971, .T. ) ;
#6439 = CARTESIAN_POINT ( 'NONE',  ( -7.714727599197334307, 2.046875000000014211, -18.62500000000064659 ) ) ;
#6440 = CARTESIAN_POINT ( 'NONE',  ( -13.49893008054767307, 67.93627681339535229, 0.1832009443085887701 ) ) ;
#6441 = CARTESIAN_POINT ( 'NONE',  ( -13.16986379959834252, -39.54374999999990337, -13.16986379960055054 ) ) ;
#6442 = CARTESIAN_POINT ( 'NONE',  ( 4.773287838552558782, 55.00798678553170618, -12.62802569744146552 ) ) ;
#6443 = CARTESIAN_POINT ( 'NONE',  ( 13.16986379960055054, -68.68124999999983515, -13.16986379959834430 ) ) ;
#6444 = CARTESIAN_POINT ( 'NONE',  ( -6.760456215069256203, 65.43070360383805451, 11.70411596025642886 ) ) ;
#6445 = DIRECTION ( 'NONE',  ( 0.000000000000000000, 0.000000000000000000, -1.000000000000000000 ) ) ;
#6446 = CARTESIAN_POINT ( 'NONE',  ( -9.396703253528214006, 35.31151048980861162, 9.692882425390839884 ) ) ;
#6447 = CARTESIAN_POINT ( 'NONE',  ( -10.92172942406178926, 20.63000000000000966, -7.935100905948389460 ) ) ;
#6448 = EDGE_LOOP ( 'NONE', ( #2153, #13085 ) ) ;
#6449 = DIRECTION ( 'NONE',  ( -0.000000000000000000, -1.000000000000000000, -0.000000000000000000 ) ) ;
#6450 = CARTESIAN_POINT ( 'NONE',  ( -3.690040334857666249, 40.31264515183992359, -12.98793614100416782 ) ) ;
#6451 = CARTESIAN_POINT ( 'NONE',  ( -12.61099646397594576, 32.10463546966393977, 4.817970500361715480 ) ) ;
#6452 = CARTESIAN_POINT ( 'NONE',  ( 0.2743714829360081597, 73.17013493549970349, -13.49759525946641858 ) ) ;
#6453 = CARTESIAN_POINT ( 'NONE',  ( -10.92172942406179104, -2.769999999999994689, 7.935100905948385908 ) ) ;
#6454 =( BOUNDED_CURVE ( )  B_SPLINE_CURVE ( 2, ( #9472, #16149, #2624, #4057, #10614, #9385, #14566, #8057, #14820, #8235, #13421, #6906, #12191 ),
 .UNSPECIFIED., .F., .T. ) 
 B_SPLINE_CURVE_WITH_KNOTS ( ( 3, 2, 2, 2, 2, 2, 3 ),
 ( 0.4861111111111111049, 0.4888888888888888729, 0.4944444444444444642, 0.5000000000000000000, 0.5055555555555555358, 0.5111111111111110716, 0.5138888888888888395 ),
 .UNSPECIFIED. ) 
 CURVE ( )  GEOMETRIC_REPRESENTATION_ITEM ( )  RATIONAL_B_SPLINE_CURVE ( ( 0.9755282581475768211, 0.9755282581475768211, 1.000000000000000000, 0.9510565162951535312, 1.000000000000000000, 0.9510565162951535312, 1.000000000000000000, 0.9510565162951535312, 1.000000000000000000, 0.9510565162951535312, 1.000000000000000000, 0.9755282581475772652, 0.9755282581475768211 ) ) 
 REPRESENTATION_ITEM ( '' )  );
#6455 = CARTESIAN_POINT ( 'NONE',  ( -0.7596481966012033071, 53.65269506995328896, 13.47926920936900608 ) ) ;
#6456 = CARTESIAN_POINT ( 'NONE',  ( -11.76794919243112325, 54.07999999999999119, 3.823638476888994386 ) ) ;
#6457 = CARTESIAN_POINT ( 'NONE',  ( -8.343458848123582072, 73.38000000000000966, 11.48378591275254124 ) ) ;
#6458 = EDGE_CURVE ( 'NONE', #1168, #12765, #12701, .T. ) ;
#6459 = CARTESIAN_POINT ( 'NONE',  ( 3.474791655989063699, 50.80483670142854891, 13.04534542254549301 ) ) ;
#6460 = CONICAL_SURFACE ( 'NONE', #5909, 9.500000000000021316, 0.7853981633974504994 ) ;
#6461 = CARTESIAN_POINT ( 'NONE',  ( -12.59156949641007728, 38.10658175097438516, 4.868567088784999441 ) ) ;
#6462 = CARTESIAN_POINT ( 'NONE',  ( 13.49495430563132992, 36.44321454405320537, -0.3851982713760790933 ) ) ;
#6463 = CARTESIAN_POINT ( 'NONE',  ( 8.043339635997652337, -42.63124999999990905, -8.043339635996302306 ) ) ;
#6464 = CARTESIAN_POINT ( 'NONE',  ( -3.081887839508138605, 74.56919532197451872, 13.14385889904788307 ) ) ;
#6465 = CARTESIAN_POINT ( 'NONE',  ( -12.13432200433486052, 77.14750715261939717, 5.916777068713412469 ) ) ;
#6466 = CARTESIAN_POINT ( 'NONE',  ( -8.343458848123578520, 60.47999999999999687, -11.48378591275254124 ) ) ;
#6467 = CARTESIAN_POINT ( 'NONE',  ( 7.499999999999999112, 108.1112172271399743, 5.064597142177447608 ) ) ;
#6468 = ORIENTED_EDGE ( 'NONE', *, *, #2212, .T. ) ;
#6469 = CARTESIAN_POINT ( 'NONE',  ( -9.520470885617717371, 16.22999999999999332, 6.917026985038133624 ) ) ;
#6470 = ORIENTED_EDGE ( 'NONE', *, *, #8177, .F. ) ;
#6471 = CARTESIAN_POINT ( 'NONE',  ( 3.636496289402157078, 56.02999999999999403, -11.19198476289190936 ) ) ;
#6472 = CARTESIAN_POINT ( 'NONE',  ( -9.552639591052204498E-13, -71.83749999999979252, 11.37500000000000178 ) ) ;
#6473 = CARTESIAN_POINT ( 'NONE',  ( 8.043339635996300530, -97.81874999999976694, 8.043339635997654113 ) ) ;
#6474 = CARTESIAN_POINT ( 'NONE',  ( -8.343458848123582072, -3.620000000000003215, 11.48378591275254124 ) ) ;
#6475 = CARTESIAN_POINT ( 'NONE',  ( 8.583537299616791572, 75.85053009153234882, -10.41983335155395451 ) ) ;
#6476 = AXIS2_PLACEMENT_3D ( 'NONE', #273, #5684, #12731 ) ;
#6477 = DIRECTION ( 'NONE',  ( 0.000000000000000000, -1.000000000000000000, 0.000000000000000000 ) ) ;
#6478 = CARTESIAN_POINT ( 'NONE',  ( -13.49999999999999822, 73.77999999999998693, -4.386415899144240349 ) ) ;
#6479 = CARTESIAN_POINT ( 'NONE',  ( -3.636496289402153081, 38.32999999999999829, -11.19198476289190936 ) ) ;
#6480 = LINE ( 'NONE', #14400, #13984 ) ;
#6481 = EDGE_CURVE ( 'NONE', #15151, #14477, #4189, .T. ) ;
#6482 = CARTESIAN_POINT ( 'NONE',  ( -11.13989584533736732, 59.21702220567828334, 7.626482110035076367 ) ) ;
#6483 = CARTESIAN_POINT ( 'NONE',  ( 9.945261256422160301, 45.07602360461397240, 9.147325197284214227 ) ) ;
#6484 = CARTESIAN_POINT ( 'NONE',  ( 13.26845858006661949, 69.34132304966905735, 2.518521654702833956 ) ) ;
#6485 = CARTESIAN_POINT ( 'NONE',  ( -18.99999999999998224, 0.000000000000000000, -1.732050807569074369 ) ) ;
#6486 = CARTESIAN_POINT ( 'NONE',  ( 12.02149203852282788, 30.65648930801207328, -6.142778965568425065 ) ) ;
#6487 = VECTOR ( 'NONE', #4163, 1000.000000000000227 ) ;
#6488 = CARTESIAN_POINT ( 'NONE',  ( -4.298585430698084409, 55.33458420718728377, -12.79766616383132671 ) ) ;
#6489 = CARTESIAN_POINT ( 'NONE',  ( -5.433699768483149839, 50.48312169129376059, 12.35834494753474289 ) ) ;
#6490 = CARTESIAN_POINT ( 'NONE',  ( 5.356475045761456499, 63.98608451589991830, -12.39185946976114927 ) ) ;
#6491 = CARTESIAN_POINT ( 'NONE',  ( 13.00839847755452894, 42.55890957469971880, -3.609942547316297823 ) ) ;
#6492 = CARTESIAN_POINT ( 'NONE',  ( 10.48980811747609998, 39.10526784545407963, 8.500966251292467746 ) ) ;
#6493 = VERTEX_POINT ( 'NONE', #5911 ) ;
#6494 = CARTESIAN_POINT ( 'NONE',  ( -7.815479942303253047, 70.47470329232851327, -11.00769136349473065 ) ) ;
#6495 = CARTESIAN_POINT ( 'NONE',  ( -7.305932770837913814, 61.45259908546214689, -11.35225092655161383 ) ) ;
#6496 = CARTESIAN_POINT ( 'NONE',  ( 7.272992578804311492, 2.880000000000001670, -10.01041549318726709 ) ) ;
#6497 = ORIENTED_EDGE ( 'NONE', *, *, #1224, .F. ) ;
#6498 = AXIS2_PLACEMENT_3D ( 'NONE', #15329, #765, #11640 ) ;
#6499 = VERTEX_POINT ( 'NONE', #1899 ) ;
#6500 = CARTESIAN_POINT ( 'NONE',  ( 13.50000000000000355, 21.58000000000000895, -4.386415899144233244 ) ) ;
#6501 = CARTESIAN_POINT ( 'NONE',  ( -7.714727599197335195, -71.80312499999982379, -18.62500000000064304 ) ) ;
#6502 = CARTESIAN_POINT ( 'NONE',  ( 2.930883425776768636, 61.07461791577657806, -13.17823006371532735 ) ) ;
#6503 = PRODUCT_DEFINITION_SHAPE ( 'NONE', 'NONE',  #8924 ) ;
#6504 = CARTESIAN_POINT ( 'NONE',  ( 12.43727753264746028, 57.23865299909770243, 5.250246734765029899 ) ) ;
#6505 = VECTOR ( 'NONE', #13445, 1000.000000000000000 ) ;
#6506 = CARTESIAN_POINT ( 'NONE',  ( 11.76794919243112680, 70.58000000000001251, -3.823638476888993942 ) ) ;
#6507 = CARTESIAN_POINT ( 'NONE',  ( -7.576616670048093940E-16, 75.67999999999999261, 12.37355403259654985 ) ) ;
#6508 = CARTESIAN_POINT ( 'NONE',  ( -0.08604155877350383452, 47.67690458564754863, 13.49999999999964295 ) ) ;
#6509 = B_SPLINE_CURVE_WITH_KNOTS ( 'NONE', 3,
 ( #11295, #682, #14192, #6094, #2076, #7586, #770, #6178, #12965, #11212, #16586, #4491, #13924, #17108, #7674, #14531, #11731, #11990, #17023, #5286, #6346, #3770, #10585, #4927, #11821, #2246, #15771, #9182, #17371, #15681, #3588, #17283, #15946, #14358, #5108, #6527, #10500, #936, #13139, #2417, #10669, #16033, #17200, #11645, #6258, #1027, #5197, #2334, #13053, #8023, #3941, #5014, #3680, #2593, #9096, #2506, #15863, #13391, #3855, #9269, #7936, #14448, #11906, #10326, #9000, #14621, #6437, #7850, #10414, #7768, #13224, #13309, #1112, #1199, #6611, #9355, #14704, #51, #16205, #10839, #2860, #9531, #5638, #14790, #12248, #6693, #14874, #5454, #13478, #4116, #6960, #2769, #12074, #17453, #8291, #9442, #16299, #8200, #5367, #5548, #8113, #13648, #13564, #142, #4027, #2680, #10752, #9618, #6873, #1455, #14969, #11020, #10932, #232, #1543, #12340, #16116, #4206, #1365, #6782, #1280, #12160, #2563, #3825, #2649, #6580, #6747, #17422, #2473, #16002, #14500, #1250, #5165, #16087, #13106, #10470, #17340, #9153, #2387, #3995, #7823, #10384, #1169, #12044, #9061, #5076, #15738, #14759, #8080, #13444, #11961, #3908, #1081, #9325, #17077, #14593, #14675, #3647, #10557, #993, #13195, #1331, #4981, #15831, #6494, #3736, #7993, #9411, #14414, #2302, #7730, #11877, #6405, #5337, #5251, #10722, #15916, #11789, #17166, #17252, #13361, #9239, #7906, #13281, #10637, #6662, #9849, #5603, #11073, #107, #1774, #198, #1511, #16535, #284, #10895, #16264, #8432, #13786, #4261, #10986, #16446, #9584, #1684, #16355, #11160, #8167 ),
 .UNSPECIFIED., .F., .F.,
 ( 4, 1, 2, 2, 1, 1, 1, 2, 2, 2, 2, 2, 2, 1, 1, 2, 2, 2, 1, 2, 2, 1, 1, 2, 1, 1, 1, 2, 2, 1, 1, 2, 2, 2, 2, 2, 1, 1, 1, 2, 2, 1, 1, 1, 2, 2, 1, 1, 1, 2, 2, 2, 2, 1, 1, 2, 2, 1, 1, 2, 2, 2, 2, 1, 2, 2, 2, 2, 2, 2, 1, 1, 2, 2, 1, 1, 1, 2, 2, 1, 2, 2, 2, 2, 1, 2, 2, 1, 2, 2, 2, 1, 1, 1, 2, 2, 1, 2, 2, 2, 2, 1, 1, 1, 1, 2, 2, 2, 2, 2, 2, 2, 2, 2, 2, 2, 1, 2, 2, 1, 1, 2, 2, 1, 1, 2, 2, 4 ),
 ( 0.1814966425150734142, 0.1816111196666974903, 0.1816397389546035024, 0.1816468937765800262, 0.1816540485985565223, 0.1816683582425095422, 0.1817255968183215664, 0.1819545511215697464, 0.1824124597280660509, 0.1833282769410587154, 0.1835572312443068677, 0.1835858505322129075, 0.1836001601761658997, 0.1836144698201189196, 0.1836717083959309438, 0.1837861855475550199, 0.1842440941540512966, 0.1844730484572994489, 0.1845302870331114731, 0.1845589063210174852, 0.1845732159649705051, 0.1845875256089234973, 0.1847020027605476011, 0.1851599113670439056, 0.1853888656702920579, 0.1855033428219161340, 0.1855319621098221461, 0.1855462717537751660, 0.1855534265757516621, 0.1855605813977281582, 0.1856178199735402101, 0.1860757285800365979, 0.1869915457930293456, 0.1874494543995257334, 0.1874780736874317455, 0.1875066929753377576, 0.1875639315511498095, 0.1876784087027739134, 0.1879073630060221212, 0.1888231802190149522, 0.1906548146450005865, 0.1911127232514970020, 0.1913416775547452098, 0.1913989161305572617, 0.1914060709525337578, 0.1914096483635220058, 0.1914132257745102539, 0.1914275354184632738, 0.1914561547063693137, 0.1915706318579935008, 0.1924864490709868314, 0.1929443576774834967, 0.1931733119807318433, 0.1932877891323560027, 0.1933450277081680824, 0.1933593373521211300, 0.1933664921740976261, 0.1933736469960741500, 0.1934022662839801898, 0.1943180834969736315, 0.1952339007099670731, 0.1952911392857791528, 0.1953197585736852204, 0.1953483778615912603, 0.1954628550132154197, 0.1956918093164637940, 0.1961497179229604870, 0.1962641950745846742, 0.1962785047185376941, 0.1962928143624907140, 0.1963214336503967539, 0.1963786722262088336, 0.1966076265294572079, 0.1970655351359539009, 0.1971800122875780881, 0.1972372508633901678, 0.1972515605073431877, 0.1972587153293197115, 0.1972658701512962076, 0.1972944894392022475, 0.1975234437424505385, 0.1979813523489470928, 0.1988971695619402569, 0.1991261238651885479, 0.1991833624410006276, 0.1992119817289066397, 0.1992406010168126795, 0.1993550781684368389, 0.1998129867749333932, 0.2016446212009196937, 0.2025604384139128300, 0.2030183470204093843, 0.2030755855962214640, 0.2031042048841275038, 0.2031185145280805238, 0.2031256693500570476, 0.2031328241720335437, 0.2032473013236579806, 0.2034762556269068545, 0.2043920728399024056, 0.2048499814464001811, 0.2049644585980246181, 0.2050216971738368366, 0.2050503164617429597, 0.2050646261056960074, 0.2050717809276725312, 0.2050789357496490550, 0.2053078900528980677, 0.2062237072658940629, 0.2066816158723920327, 0.2069105701756410454, 0.2070250473272655378, 0.2070822859030777841, 0.2071395244788900303, 0.2075974330853880279, 0.2078263873886370128, 0.2079408645402615052, 0.2079981031160737515, 0.2080124127600268269, 0.2080267224039798746, 0.2080553416918859977, 0.2089711589048821316, 0.2090283974806943779, 0.2090856360565066518, 0.2092001132081311443, 0.2094290675113801847, 0.2098869761178782378, 0.2108027933308743440 ),
 .UNSPECIFIED. ) ;
#6510 = CARTESIAN_POINT ( 'NONE',  ( -8.891200544363830713E-16, 40.67999999999999261, 13.50000000000000000 ) ) ;
#6511 = CARTESIAN_POINT ( 'NONE',  ( 7.500000000000000888, -18.00000000000000355, -2.204364238465235822E-15 ) ) ;
#6512 = CARTESIAN_POINT ( 'NONE',  ( -11.37500000000000000, -24.97499999999994102, -9.545674412382054647E-13 ) ) ;
#6513 = CARTESIAN_POINT ( 'NONE',  ( 10.92172942406178926, 44.13000000000000256, 7.935100905948387684 ) ) ;
#6514 = CARTESIAN_POINT ( 'NONE',  ( 5.336470388020742028, 33.98688528483218363, -12.40243878204504213 ) ) ;
#6515 = CARTESIAN_POINT ( 'NONE',  ( -2.994701108386524258, 73.28771383196766465, -13.16632730457292766 ) ) ;
#6516 = ORIENTED_EDGE ( 'NONE', *, *, #2487, .T. ) ;
#6517 = ORIENTED_EDGE ( 'NONE', *, *, #14361, .F. ) ;
#6518 = CARTESIAN_POINT ( 'NONE',  ( 3.636496289402157078, 80.03000000000000114, -11.19198476289190936 ) ) ;
#6519 = EDGE_LOOP ( 'NONE', ( #10846, #1190, #11722, #1123 ) ) ;
#6520 = CARTESIAN_POINT ( 'NONE',  ( -8.343458848123576743, 13.48000000000001641, -11.48378591275254301 ) ) ;
#6521 = CARTESIAN_POINT ( 'NONE',  ( 7.714727599200456254, -10.37187499999999396, -18.62499999999935341 ) ) ;
#6522 = EDGE_CURVE ( 'NONE', #12765, #3761, #10730, .T. ) ;
#6523 = CARTESIAN_POINT ( 'NONE',  ( -5.526118766865936394, 44.47964708879426610, 12.32381976411106450 ) ) ;
#6524 = CARTESIAN_POINT ( 'NONE',  ( -7.499999999999996447, -25.28385182205995463, 8.084116494856628421 ) ) ;
#6525 = CARTESIAN_POINT ( 'NONE',  ( 11.59702038864718432, 66.68748371943325992, -6.910806977644125659 ) ) ;
#6526 = CARTESIAN_POINT ( 'NONE',  ( -13.49999999999999822, 40.78000000000000114, -4.386415899144240349 ) ) ;
#6527 = CARTESIAN_POINT ( 'NONE',  ( -4.555328311572941935, 71.51607439978332081, 12.70834120064674622 ) ) ;
#6528 = PRODUCT_DEFINITION_FORMATION_WITH_SPECIFIED_SOURCE ( 'ANY', '', #2950, .NOT_KNOWN. ) ;
#6529 = CARTESIAN_POINT ( 'NONE',  ( -13.16986379960055231, -93.65624999999977263, 13.16986379959834252 ) ) ;
#6530 = CARTESIAN_POINT ( 'NONE',  ( -12.69503808151269553, 68.09607240394507244, 4.594974419746471028 ) ) ;
#6531 = CARTESIAN_POINT ( 'NONE',  ( -7.714727599197334307, -14.60312499999994706, -18.62500000000064659 ) ) ;
#6532 = CARTESIAN_POINT ( 'NONE',  ( 2.474201151127992215, 55.09108309819342963, -13.27610207924121255 ) ) ;
#6533 = CARTESIAN_POINT ( 'NONE',  ( -7.714727599197335195, -88.45312499999978684, -18.62500000000064304 ) ) ;
#6534 = CARTESIAN_POINT ( 'NONE',  ( -12.86040510649366553, 65.07770000608704208, 4.111097590322251527 ) ) ;
#6535 = CARTESIAN_POINT ( 'NONE',  ( -6.936718818989325186, 35.42298707049641848, 11.58157915692249773 ) ) ;
#6536 = ORIENTED_EDGE ( 'NONE', *, *, #6196, .F. ) ;
#6537 = FACE_OUTER_BOUND ( 'NONE', #16577, .T. ) ;
#6538 = CARTESIAN_POINT ( 'NONE',  ( 7.272992578804311492, 26.88000000000001677, -10.01041549318726709 ) ) ;
#6539 = CARTESIAN_POINT ( 'NONE',  ( -7.993062784379826979, 31.48258056696385410, -10.87940591478879604 ) ) ;
#6540 = CARTESIAN_POINT ( 'NONE',  ( 0.000000000000000000, 9.999999999999998224, 0.000000000000000000 ) ) ;
#6541 = CARTESIAN_POINT ( 'NONE',  ( 11.48106618170696080, 60.16469814098914526, 7.105216182321891338 ) ) ;
#6542 = CARTESIAN_POINT ( 'NONE',  ( 13.49999999999999822, -7.720000000000004192, 4.386415899144237684 ) ) ;
#6543 = CARTESIAN_POINT ( 'NONE',  ( -7.133837838234538431, 53.41470899139449102, 11.46116927770655813 ) ) ;
#6544 = CARTESIAN_POINT ( 'NONE',  ( 3.636496289402157078, 53.03000000000000114, -11.19198476289190936 ) ) ;
#6545 = CARTESIAN_POINT ( 'NONE',  ( 10.92172942406178926, 77.13000000000000966, 7.935100905948387684 ) ) ;
#6546 = CARTESIAN_POINT ( 'NONE',  ( 4.773616553820369646, 50.85195731075037884, 12.62846895061231578 ) ) ;
#6547 = CARTESIAN_POINT ( 'NONE',  ( -9.258348693882576086, 37.54127912305889936, -9.843850005556705085 ) ) ;
#6548 = CARTESIAN_POINT ( 'NONE',  ( 13.28445700308491162, 36.34535166002273598, 2.405321636251910977 ) ) ;
#6549 = CARTESIAN_POINT ( 'NONE',  ( -8.043339635996300530, -46.79374999999990337, -8.043339635997652337 ) ) ;
#6550 = CARTESIAN_POINT ( 'NONE',  ( 1.900613283894434735, 1.622906826104706601, 12.00000000000000000 ) ) ;
#6551 = CARTESIAN_POINT ( 'NONE',  ( -6.401350755636498135, 77.44499155070386109, 11.88582777253868450 ) ) ;
#6552 = CARTESIAN_POINT ( 'NONE',  ( -12.79004503783874469, 79.77371121109450769, -4.343132741677108832 ) ) ;
#6553 = CARTESIAN_POINT ( 'NONE',  ( -11.76794919243112325, 13.07999999999999829, 3.823638476888994386 ) ) ;
#6554 = CARTESIAN_POINT ( 'NONE',  ( 7.500000000000000000, 104.2024577724304208, 9.199283337799339932 ) ) ;
#6555 = ORIENTED_EDGE ( 'NONE', *, *, #16241, .T. ) ;
#6556 = CARTESIAN_POINT ( 'NONE',  ( 11.76794919243112325, 2.280000000000006466, 3.823638476888996163 ) ) ;
#6557 = EDGE_LOOP ( 'NONE', ( #12937, #6882, #16005, #2648 ) ) ;
#6558 = CARTESIAN_POINT ( 'NONE',  ( -7.272992578804307939, 53.47999999999998977, -10.01041549318727064 ) ) ;
#6559 = CARTESIAN_POINT ( 'NONE',  ( 8.043339635997652337, -78.08124999999978400, -8.043339635996304082 ) ) ;
#6560 = CARTESIAN_POINT ( 'NONE',  ( 6.475374228414382927, 9.912830568698879574, 12.09076339992581417 ) ) ;
#6561 = CARTESIAN_POINT ( 'NONE',  ( 13.49999999999999822, -5.720000000000003304, 4.386415899144237684 ) ) ;
#6562 = EDGE_CURVE ( 'NONE', #16381, #14613, #1644, .T. ) ;
#6563 = CARTESIAN_POINT ( 'NONE',  ( 6.109412881612292345, 75.95670156276325713, -12.03862480236976396 ) ) ;
#6564 = CARTESIAN_POINT ( 'NONE',  ( 7.714727599197339636, -96.77812499999977547, 18.62500000000063949 ) ) ;
#6565 = CARTESIAN_POINT ( 'NONE',  ( -13.50000000000000000, 76.92999999999999261, -3.306546357697853733E-15 ) ) ;
#6566 = CARTESIAN_POINT ( 'NONE',  ( -11.76794919243112325, 44.92999999999999972, -2.882316262207890869E-15 ) ) ;
#6567 = DIRECTION ( 'NONE',  ( -0.000000000000000000, 1.000000000000000000, -0.000000000000000000 ) ) ;
#6568 = CARTESIAN_POINT ( 'NONE',  ( -11.18263218352950972, 58.64562392974652028, -7.562986225119091799 ) ) ;
#6569 = CARTESIAN_POINT ( 'NONE',  ( 13.49528878454824543, 45.41772704297711272, 0.3573627978170749731 ) ) ;
#6570 = CARTESIAN_POINT ( 'NONE',  ( 13.10377846605443963, 69.54542809245315027, -3.246696344792387556 ) ) ;
#6571 = CIRCLE ( 'NONE', #7984, 12.00000000000000178 ) ;
#6572 = CARTESIAN_POINT ( 'NONE',  ( 1.653273178848926472E-15, 80.93000000000000682, 13.50000000000000000 ) ) ;
#6573 = CARTESIAN_POINT ( 'NONE',  ( 9.999999999999902300, 0.000000000000000000, 17.32050807568882789 ) ) ;
#6574 = CARTESIAN_POINT ( 'NONE',  ( -10.18807947666135583, 55.58911967552339917, -8.857645364605666316 ) ) ;
#6575 = CARTESIAN_POINT ( 'NONE',  ( -10.93185410481415154, 50.22943847104855308, 7.921438598450179391 ) ) ;
#6576 = CARTESIAN_POINT ( 'NONE',  ( 11.49298963318043398, 63.69447171356610937, -7.082473735879659671 ) ) ;
#6577 = CARTESIAN_POINT ( 'NONE',  ( 8.081592316167094836, 42.87346269304677548, -10.81406279893415068 ) ) ;
#6578 = CARTESIAN_POINT ( 'NONE',  ( 11.13323897052192635, 39.14259498289401762, 7.635513019236351617 ) ) ;
#6579 = ORIENTED_EDGE ( 'NONE', *, *, #13611, .T. ) ;
#6580 = CARTESIAN_POINT ( 'NONE',  ( -13.38634760227498255, 70.86891057379173731, -1.749485324747906301 ) ) ;
#6581 = CARTESIAN_POINT ( 'NONE',  ( -2.555879417051283298, 61.27177513301734990, -13.26191791090011307 ) ) ;
#6582 = CARTESIAN_POINT ( 'NONE',  ( 7.272992578804308828, 4.980000000000008420, 10.01041549318726709 ) ) ;
#6583 = EDGE_LOOP ( 'NONE', ( #2849, #10939, #11633, #6771 ) ) ;
#6584 = VERTEX_POINT ( 'NONE', #8652 ) ;
#6585 = CARTESIAN_POINT ( 'NONE',  ( -10.92172942406178926, 19.63000000000000966, -7.935100905948389460 ) ) ;
#6586 = CARTESIAN_POINT ( 'NONE',  ( -7.714727599200467800, -78.04687499999982947, 18.62499999999934630 ) ) ;
#6587 = CARTESIAN_POINT ( 'NONE',  ( 3.060653757609212544, 47.79012880483755055, 13.14927094501084426 ) ) ;
#6588 = TOROIDAL_SURFACE ( 'NONE', #6022, 6.000000000000001776, 6.000000000000000000 ) ;
#6589 = CARTESIAN_POINT ( 'NONE',  ( 2.337253843264979203, 71.76409061300877568, 13.29619868658769199 ) ) ;
#6590 = CARTESIAN_POINT ( 'NONE',  ( 13.35987737257807950, 57.49792048163389779, -1.940069495529155308 ) ) ;
#6591 = CARTESIAN_POINT ( 'NONE',  ( 7.272992578804308828, 72.98000000000000398, 10.01041549318726709 ) ) ;
#6592 = CARTESIAN_POINT ( 'NONE',  ( 11.76794919243112325, 76.28000000000000114, 3.823638476888996607 ) ) ;
#6593 = CARTESIAN_POINT ( 'NONE',  ( -9.858871623890049563, 47.28812877695573746, 9.222456157666663046 ) ) ;
#6594 = LINE ( 'NONE', #9513, #14081 ) ;
#6595 = CARTESIAN_POINT ( 'NONE',  ( -1.688033560168326508, 9.999999999999996447, -13.00620140183451490 ) ) ;
#6596 = CARTESIAN_POINT ( 'NONE',  ( 4.711679271994909435, -36.42187499999990763, -11.37499999999960387 ) ) ;
#6597 = AXIS2_PLACEMENT_3D ( 'NONE', #9393, #16248, #2633 ) ;
#6598 = FACE_OUTER_BOUND ( 'NONE', #2940, .T. ) ;
#6599 = CARTESIAN_POINT ( 'NONE',  ( 5.806605737915351284, 33.96866633168072269, -12.18742560399044983 ) ) ;
#6600 = CARTESIAN_POINT ( 'NONE',  ( -3.655908334455305386, 73.31145551481743894, -12.99555118694178724 ) ) ;
#6601 = ORIENTED_EDGE ( 'NONE', *, *, #15801, .T. ) ;
#6602 = ORIENTED_EDGE ( 'NONE', *, *, #3449, .T. ) ;
#6603 = CARTESIAN_POINT ( 'NONE',  ( 11.76794919243112325, 73.42999999999999261, 1.441158131103945434E-15 ) ) ;
#6604 = ORIENTED_EDGE ( 'NONE', *, *, #5085, .F. ) ;
#6605 = EDGE_CURVE ( 'NONE', #13128, #15397, #2389, .T. ) ;
#6606 = CARTESIAN_POINT ( 'NONE',  ( -12.70590379749083532, 41.09495175222023278, 4.565257769830444623 ) ) ;
#6607 = CARTESIAN_POINT ( 'NONE',  ( -8.043339635996300530, -80.09374999999982947, -8.043339635997652337 ) ) ;
#6608 = CARTESIAN_POINT ( 'NONE',  ( -1.180642086793956880, 44.63755760315241616, 13.45088169940935785 ) ) ;
#6609 = CARTESIAN_POINT ( 'NONE',  ( 9.835827272001290922, 8.007293614239925361, 15.31970530204991121 ) ) ;
#6610 = CARTESIAN_POINT ( 'NONE',  ( 8.343458848123583849, 39.88000000000000256, -11.48378591275253768 ) ) ;
#6611 = CARTESIAN_POINT ( 'NONE',  ( -11.84785472851091725, 71.16967805033135619, 6.471368726115286130 ) ) ;
#6612 = CARTESIAN_POINT ( 'NONE',  ( 13.16986379960055409, -61.43124999999983515, -13.16986379959834430 ) ) ;
#6613 = CARTESIAN_POINT ( 'NONE',  ( -13.49960910270157477, 67.93362544972310957, 0.1058906348414896115 ) ) ;
#6614 = CARTESIAN_POINT ( 'NONE',  ( 18.62500000000064304, -84.29062499999983515, -7.714727599197335195 ) ) ;
#6615 = CARTESIAN_POINT ( 'NONE',  ( 4.837186686068091213, 55.00564863163254614, -12.60363724258546725 ) ) ;
#6616 = CARTESIAN_POINT ( 'NONE',  ( -18.99999999999998224, 7.773118517290098062, -1.732050807569074147 ) ) ;
#6617 = CARTESIAN_POINT ( 'NONE',  ( -13.47566967663552262, 64.96175637022594174, 0.9213295838320114672 ) ) ;
#6618 = CARTESIAN_POINT ( 'NONE',  ( -7.866623628157809911, 35.38328011712205523, 10.98017150749901738 ) ) ;
#6619 = CARTESIAN_POINT ( 'NONE',  ( 10.92172942406178926, 22.13000000000000966, 7.935100905948385908 ) ) ;
#6620 = ORIENTED_EDGE ( 'NONE', *, *, #14405, .F. ) ;
#6621 = CARTESIAN_POINT ( 'NONE',  ( 8.343458848123580296, 49.97999999999999687, 11.48378591275253768 ) ) ;
#6622 = DIRECTION ( 'NONE',  ( 0.000000000000000000, 0.000000000000000000, -1.000000000000000000 ) ) ;
#6623 = CARTESIAN_POINT ( 'NONE',  ( -10.15547274497371077, 31.58743970881114294, -8.894744516544626833 ) ) ;
#6624 = CARTESIAN_POINT ( 'NONE',  ( -7.499999999999998224, -8.000000000000000000, -22.50000000000000355 ) ) ;
#6625 = CARTESIAN_POINT ( 'NONE',  ( 2.279995255611139653E-15, -11.81999999999999851, -12.37355403259654985 ) ) ;
#6626 = CARTESIAN_POINT ( 'NONE',  ( 4.946212110863060119, 59.85840281924108552, 12.56136872037263075 ) ) ;
#6627 = CARTESIAN_POINT ( 'NONE',  ( -4.171729424061791036, -5.469999999999995310, 12.83926296998457239 ) ) ;
#6628 = CARTESIAN_POINT ( 'NONE',  ( -9.936413839488240640, 53.28410195231833058, 9.138806663926128948 ) ) ;
#6629 = CARTESIAN_POINT ( 'NONE',  ( -7.272992578804310604, 51.37999999999998835, 10.01041549318726709 ) ) ;
#6630 = PRODUCT_CONTEXT ( 'NONE', #3256, 'mechanical' ) ;
#6631 = CARTESIAN_POINT ( 'NONE',  ( 4.171729424061789260, 70.82999999999999829, 12.83926296998457417 ) ) ;
#6632 = CARTESIAN_POINT ( 'NONE',  ( 3.336094116535059495, 50.79992621253678919, 13.08131499243033602 ) ) ;
#6633 = CARTESIAN_POINT ( 'NONE',  ( -12.98164777139678527, 37.79751183502862233, -3.705885770400368706 ) ) ;
#6634 = AXIS2_PLACEMENT_3D ( 'NONE', #9871, #4104, #13553 ) ;
#6635 = CARTESIAN_POINT ( 'NONE',  ( 9.257065025830906180, 36.04160388237846746, 9.826378808067678605 ) ) ;
#6636 = CARTESIAN_POINT ( 'NONE',  ( -4.711679271993001628, -95.70312499999977263, -11.37500000000039613 ) ) ;
#6637 = CARTESIAN_POINT ( 'NONE',  ( 3.708203932499371192, 2.896025403784442620, -11.41267819554184548 ) ) ;
#6638 = CARTESIAN_POINT ( 'NONE',  ( -13.04317161032976813, 77.05446084332930923, 3.489292788701963577 ) ) ;
#6639 = CARTESIAN_POINT ( 'NONE',  ( -7.311605416996860285, 79.45288813049690191, -11.35076817521309067 ) ) ;
#6640 = CARTESIAN_POINT ( 'NONE',  ( 7.500000000000000000, 103.1885367479068663, 9.367496997597603681 ) ) ;
#6641 = CARTESIAN_POINT ( 'NONE',  ( -7.409984580736203970E-16, 1.680000000000003491, 12.37355403259654985 ) ) ;
#6642 = CARTESIAN_POINT ( 'NONE',  ( 3.636496289402154414, 42.82999999999999829, 11.19198476289190936 ) ) ;
#6643 = CARTESIAN_POINT ( 'NONE',  ( 11.37500000000000178, -75.99999999999980105, 9.531744055041752924E-13 ) ) ;
#6644 = CARTESIAN_POINT ( 'NONE',  ( -1.564113515457998572E-12, -12.48749999999997051, 18.62500000000000000 ) ) ;
#6645 = CARTESIAN_POINT ( 'NONE',  ( 2.621994543952811015E-15, -4.820000000000002949, -14.19474002721660355 ) ) ;
#6646 = FACE_BOUND ( 'NONE', #12655, .T. ) ;
#6647 = CARTESIAN_POINT ( 'NONE',  ( 10.86178057370645611, 75.73342452336723341, -8.018662730335858413 ) ) ;
#6648 = CARTESIAN_POINT ( 'NONE',  ( 3.780205736804012180E-08, 55.17999999864077409, -13.50000000000000000 ) ) ;
#6649 = CARTESIAN_POINT ( 'NONE',  ( -3.636496289402155746, 39.52999999999999403, 11.19198476289190936 ) ) ;
#6650 = CARTESIAN_POINT ( 'NONE',  ( -7.060065731298120539, 41.41782043715235062, 11.50681685508514462 ) ) ;
#6651 = CARTESIAN_POINT ( 'NONE',  ( -8.735628014122772456, 58.51658140302173905, -10.29271241388457092 ) ) ;
#6652 = ADVANCED_FACE ( 'NONE', ( #13831 ), #13222, .T. ) ;
#6653 = DIRECTION ( 'NONE',  ( -0.000000000000000000, -1.000000000000000000, -0.000000000000000000 ) ) ;
#6654 = DIRECTION ( 'NONE',  ( -0.000000000000000000, 1.000000000000000000, -0.000000000000000000 ) ) ;
#6655 = CARTESIAN_POINT ( 'NONE',  ( 7.500000000000001776, 88.93000000000000682, -12.00000000000000178 ) ) ;
#6656 = CARTESIAN_POINT ( 'NONE',  ( -11.13669601958308597, 55.64279577809516297, -7.630683010739963912 ) ) ;
#6657 = CARTESIAN_POINT ( 'NONE',  ( -13.46035977005674766, 49.89415119664435849, -1.037902563494175867 ) ) ;
#6658 = CARTESIAN_POINT ( 'NONE',  ( 12.58047463934393662, 63.60811412330714631, -4.909781203544855366 ) ) ;
#6659 = CARTESIAN_POINT ( 'NONE',  ( 11.34081891867551306, 42.70472919525936817, -7.328857843363596025 ) ) ;
#6660 = CARTESIAN_POINT ( 'NONE',  ( 13.48360322846664161, 39.45292921673981112, -0.6651861330368826764 ) ) ;
#6661 = VERTEX_POINT ( 'NONE', #16489 ) ;
#6662 = CARTESIAN_POINT ( 'NONE',  ( -4.529881605775227804, 70.34304711494489482, -12.71783548896780403 ) ) ;
#6663 = ORIENTED_EDGE ( 'NONE', *, *, #2092, .F. ) ;
#6664 = ORIENTED_EDGE ( 'NONE', *, *, #12732, .F. ) ;
#6665 = CARTESIAN_POINT ( 'NONE',  ( -13.50000000000000000, 22.93000000000000682, -3.469446951953614189E-15 ) ) ;
#6666 = CARTESIAN_POINT ( 'NONE',  ( -18.62500000000064659, -59.31562499999985505, 7.714727599197335195 ) ) ;
#6667 = CARTESIAN_POINT ( 'NONE',  ( 4.755586391641281274, 61.00868452792411034, -12.63465254569289975 ) ) ;
#6668 = VECTOR ( 'NONE', #1310, 1000.000000000000000 ) ;
#6669 = CARTESIAN_POINT ( 'NONE',  ( -8.549982208541774191E-16, 12.67999999999999794, 14.19474002721660355 ) ) ;
#6670 = CARTESIAN_POINT ( 'NONE',  ( 2.286894564728605861, 71.76228337285282066, 13.30503304841837497 ) ) ;
#6671 = CARTESIAN_POINT ( 'NONE',  ( 12.40506120401485646, 57.23570088601564265, 5.326196437455172017 ) ) ;
#6672 = CARTESIAN_POINT ( 'NONE',  ( 2.272985001014427788E-15, 65.18000000000000682, -12.37355403259654985 ) ) ;
#6673 = CARTESIAN_POINT ( 'NONE',  ( -7.272992578804310604, 72.38000000000000966, 10.01041549318726709 ) ) ;
#6674 = CARTESIAN_POINT ( 'NONE',  ( -3.822134760076489890, 47.54257014335207998, 12.94763724393711968 ) ) ;
#6675 = CARTESIAN_POINT ( 'NONE',  ( -8.291044507619272909E-14, 45.17999999999999972, -13.50000000000000000 ) ) ;
#6676 = EDGE_CURVE ( 'NONE', #13814, #8520, #16368, .T. ) ;
#6677 = CARTESIAN_POINT ( 'NONE',  ( 3.892042677208999546, -100.0000000000000284, 14.96341192791908092 ) ) ;
#6678 = CARTESIAN_POINT ( 'NONE',  ( -7.499999999999996447, -18.00000000000000355, -2.204364238465235822E-15 ) ) ;
#6679 = CARTESIAN_POINT ( 'NONE',  ( -4.711679271993004292, -21.85312499999995239, -11.37500000000039435 ) ) ;
#6680 = AXIS2_PLACEMENT_3D ( 'NONE', #8423, #3357, #361 ) ;
#6681 = DIRECTION ( 'NONE',  ( 0.4999999999999945599, 0.000000000000000000, 0.8660254037844418162 ) ) ;
#6682 = CARTESIAN_POINT ( 'NONE',  ( 12.88504001644114538, 33.57466858618573013, -4.031382377887867463 ) ) ;
#6683 = CARTESIAN_POINT ( 'NONE',  ( -2.291594122932853139, 73.26239727050499084, -13.30408214462689820 ) ) ;
#6684 = VERTEX_POINT ( 'NONE', #6088 ) ;
#6685 = ORIENTED_EDGE ( 'NONE', *, *, #7934, .F. ) ;
#6686 = CARTESIAN_POINT ( 'NONE',  ( 3.636496289402157078, 74.03000000000000114, -11.19198476289190936 ) ) ;
#6687 = ORIENTED_EDGE ( 'NONE', *, *, #6778, .T. ) ;
#6688 = CARTESIAN_POINT ( 'NONE',  ( 18.62500000000000000, -7.250000000000001776, 1.560692158462880521E-12 ) ) ;
#6689 = CARTESIAN_POINT ( 'NONE',  ( -7.582614570348264138, 44.39550065529663669, 11.16986078532532645 ) ) ;
#6690 = CARTESIAN_POINT ( 'NONE',  ( -7.499999999999995559, -27.80914044117234596, -0.5315352956498873294 ) ) ;
#6691 = CIRCLE ( 'NONE', #1584, 8.999999999999994671 ) ;
#6692 = CARTESIAN_POINT ( 'NONE',  ( 4.171729424061791924, 46.02999999999999403, -12.83926296998457239 ) ) ;
#6693 = CARTESIAN_POINT ( 'NONE',  ( -12.92401890517933261, 71.06980940734364083, 3.901267114863464336 ) ) ;
#6694 = EDGE_CURVE ( 'NONE', #17318, #9628, #2753, .T. ) ;
#6695 = CARTESIAN_POINT ( 'NONE',  ( 18.62500000000000000, -42.69999999999988205, 1.560692158462880521E-12 ) ) ;
#6696 = CARTESIAN_POINT ( 'NONE',  ( -13.41621384453693189, 67.98230079670533144, 1.502188851297376671 ) ) ;
#6697 = CARTESIAN_POINT ( 'NONE',  ( 13.16986379959834075, -81.16874999999980389, 13.16986379960055231 ) ) ;
#6698 = CARTESIAN_POINT ( 'NONE',  ( 13.49861495593725635, 54.43666664097244023, -0.1944882449894331511 ) ) ;
#6699 = CARTESIAN_POINT ( 'NONE',  ( -13.16986379960055231, -77.00624999999982379, 13.16986379959834252 ) ) ;
#6700 = PRODUCT ( 'MAT-049', 'MAT-049', '', ( #5217 ) ) ;
#6701 = CARTESIAN_POINT ( 'NONE',  ( -12.68351458231185447, 65.09718742194731078, 4.623735391779430159 ) ) ;
#6702 = CARTESIAN_POINT ( 'NONE',  ( -12.58659164438495104, 35.10707630348271380, 4.881418642039425215 ) ) ;
#6703 = CARTESIAN_POINT ( 'NONE',  ( -8.343458848123582072, 21.37999999999999901, 11.48378591275254124 ) ) ;
#6704 = ORIENTED_EDGE ( 'NONE', *, *, #2113, .T. ) ;
#6705 = LINE ( 'NONE', #1468, #5041 ) ;
#6706 =( BOUNDED_CURVE ( )  B_SPLINE_CURVE ( 2, ( #11543, #16920, #5438, #16187, #12061, #15932, #14430, #10571, #14607, #9254, #9427, #17438, #7747 ),
 .UNSPECIFIED., .F., .F. ) 
 B_SPLINE_CURVE_WITH_KNOTS ( ( 3, 2, 2, 2, 2, 2, 3 ),
 ( 0.9305555555555555802, 0.9333333333333333481, 0.9388888888888888840, 0.9444444444444444198, 0.9499999999999999556, 0.9555555555555556024, 0.9583333333333333703 ),
 .UNSPECIFIED. ) 
 CURVE ( )  GEOMETRIC_REPRESENTATION_ITEM ( )  RATIONAL_B_SPLINE_CURVE ( ( 0.9755282581475768211, 0.9755282581475768211, 1.000000000000000000, 0.9510565162951535312, 1.000000000000000000, 0.9510565162951535312, 1.000000000000000000, 0.9510565162951535312, 1.000000000000000000, 0.9510565162951535312, 1.000000000000000000, 0.9755282581475768211, 0.9755282581475768211 ) ) 
 REPRESENTATION_ITEM ( '' )  );
#6707 = CARTESIAN_POINT ( 'NONE',  ( -2.700228618987395190, 31.27709026527809044, -13.22723019811440714 ) ) ;
#6708 = CARTESIAN_POINT ( 'NONE',  ( 4.609769263287132546, 73.01405650375669154, -12.68860813546349142 ) ) ;
#6709 = CARTESIAN_POINT ( 'NONE',  ( 18.99999999999999289, 0.000000000000000000, 1.732050807568941586 ) ) ;
#6710 = CARTESIAN_POINT ( 'NONE',  ( -13.50000000000000000, -6.069999999999999396, -3.469446951953614189E-15 ) ) ;
#6711 = B_SPLINE_CURVE_WITH_KNOTS ( 'NONE', 3,
 ( #2332, #13051, #15677, #12962 ),
 .UNSPECIFIED., .F., .F.,
 ( 4, 4 ),
 ( 2.383248697750600941E-07, 0.007646667935218598965 ),
 .UNSPECIFIED. ) ;
#6712 = CARTESIAN_POINT ( 'NONE',  ( -10.28587142665795362, 53.26568820729779219, 8.746296120241217054 ) ) ;
#6713 = CARTESIAN_POINT ( 'NONE',  ( 2.272985001014427788E-15, 47.17999999999999972, -12.37355403259654985 ) ) ;
#6714 = PRODUCT_CONTEXT ( 'NONE', #4739, 'mechanical' ) ;
#6715 = CARTESIAN_POINT ( 'NONE',  ( 10.92172942406178926, 65.12999999999999545, 7.935100905948387684 ) ) ;
#6716 = CARTESIAN_POINT ( 'NONE',  ( 12.94092419851276610, 51.29169664346532898, 3.859288104999398783 ) ) ;
#6717 = CARTESIAN_POINT ( 'NONE',  ( -6.877963339358277750, 37.43436270134902344, -11.62861394030559481 ) ) ;
#6718 = CARTESIAN_POINT ( 'NONE',  ( 8.740290627326368522, 36.01677850278021964, 10.29110420094504086 ) ) ;
#6719 = CARTESIAN_POINT ( 'NONE',  ( -18.62500000000000000, -15.57499999999998153, -1.562973063126292757E-12 ) ) ;
#6720 = CARTESIAN_POINT ( 'NONE',  ( -6.897567406690312986, 74.42478730465043668, 11.61684038191101642 ) ) ;
#6721 = CARTESIAN_POINT ( 'NONE',  ( -13.32725792319063274, 77.00693031600384586, 2.197311418460218491 ) ) ;
#6722 = CARTESIAN_POINT ( 'NONE',  ( -10.87722630759161824, 80.23258579900503662, 7.996187592776850650 ) ) ;
#6723 = CARTESIAN_POINT ( 'NONE',  ( -9.520470885617717371, 13.23000000000001997, 6.917026985038133624 ) ) ;
#6724 = CARTESIAN_POINT ( 'NONE',  ( 7.500000000000000000, 107.5003227710673315, 6.479247348114224536 ) ) ;
#6725 = CYLINDRICAL_SURFACE ( 'NONE', #9504, 12.00000000000000178 ) ;
#6726 = CARTESIAN_POINT ( 'NONE',  ( 3.636496289402157078, 0.03000000000000224709, -11.19198476289190936 ) ) ;
#6727 = CARTESIAN_POINT ( 'NONE',  ( 2.272985001014427393E-15, 50.17999999999999261, -12.37355403259654807 ) ) ;
#6728 = CARTESIAN_POINT ( 'NONE',  ( -11.37500000000000000, -24.97499999999994102, -9.545674412382054647E-13 ) ) ;
#6729 = CARTESIAN_POINT ( 'NONE',  ( 1.561832610794586538E-12, -4.162499999999989875, -18.62500000000000000 ) ) ;
#6730 = CARTESIAN_POINT ( 'NONE',  ( -8.549982208541774191E-16, -6.320000000000004725, 14.19474002721660355 ) ) ;
#6731 = CARTESIAN_POINT ( 'NONE',  ( 8.375056734751542109, 9.999950376471138824, 10.58801762894534271 ) ) ;
#6732 = CARTESIAN_POINT ( 'NONE',  ( 9.387778834394914895, 75.81219621400516928, -9.711846743374673352 ) ) ;
#6733 = ADVANCED_FACE ( 'NONE', ( #7761 ), #4747, .T. ) ;
#6734 = CARTESIAN_POINT ( 'NONE',  ( 6.750022565184456980, 31.92926174983938026, 11.69132992304556495 ) ) ;
#6735 = CARTESIAN_POINT ( 'NONE',  ( 2.272985001014427788E-15, 44.17999999999998550, -12.37355403259654985 ) ) ;
#6736 = CARTESIAN_POINT ( 'NONE',  ( -6.920156336968187105, 41.42368190141654338, 11.59162295123014097 ) ) ;
#6737 = CARTESIAN_POINT ( 'NONE',  ( -5.810482910230065023, 58.39149269753883686, -12.18558815465718936 ) ) ;
#6738 = CARTESIAN_POINT ( 'NONE',  ( -12.00000000000000178, 9.796025403784433649, -2.718289652585035561E-15 ) ) ;
#6739 = CARTESIAN_POINT ( 'NONE',  ( 2.785879211291982797E-06, 6.680077384874748780, 13.49999999999942979 ) ) ;
#6740 = CARTESIAN_POINT ( 'NONE',  ( 0.000000000000000000, 80.93000000000000682, 0.000000000000000000 ) ) ;
#6741 = DIRECTION ( 'NONE',  ( 0.000000000000000000, -1.000000000000000000, 0.000000000000000000 ) ) ;
#6742 = CARTESIAN_POINT ( 'NONE',  ( -10.13962047673653899, 49.58657935891523749, -8.912807818290596984 ) ) ;
#6743 = CARTESIAN_POINT ( 'NONE',  ( 13.36848944045340026, 63.49574276624128544, -1.879770406124993354 ) ) ;
#6744 = CARTESIAN_POINT ( 'NONE',  ( 8.526517230384889956, 42.85320048867875187, -10.46736331332614611 ) ) ;
#6745 = CARTESIAN_POINT ( 'NONE',  ( 5.574008873715639467, 38.88201036329166982, 12.30346572087647772 ) ) ;
#6746 = ORIENTED_EDGE ( 'NONE', *, *, #17277, .F. ) ;
#6747 = CARTESIAN_POINT ( 'NONE',  ( -13.37563197002901028, 70.86603882634364027, -1.829879408878430036 ) ) ;
#6748 = CARTESIAN_POINT ( 'NONE',  ( -11.37500000000000000, -8.324999999999979750, -9.545674412382054647E-13 ) ) ;
#6749 = ORIENTED_EDGE ( 'NONE', *, *, #6694, .T. ) ;
#6750 = ORIENTED_EDGE ( 'NONE', *, *, #9376, .T. ) ;
#6751 = CARTESIAN_POINT ( 'NONE',  ( 13.49999999999999822, 18.28000000000001180, 4.386415899144237684 ) ) ;
#6752 = CARTESIAN_POINT ( 'NONE',  ( 7.714727599197338748, -63.47812499999984226, 18.62500000000063949 ) ) ;
#6753 = ADVANCED_FACE ( 'NONE', ( #2070 ), #7581, .F. ) ;
#6754 = CARTESIAN_POINT ( 'NONE',  ( 9.300701112953893457, 60.81627165076186259, -9.785047430583880157 ) ) ;
#6755 = CARTESIAN_POINT ( 'NONE',  ( -8.549982208541774191E-16, 9.680000000000003268, 14.19474002721660355 ) ) ;
#6756 = CARTESIAN_POINT ( 'NONE',  ( 2.493575575080797968, 71.76962337619772825, 13.26771539037355119 ) ) ;
#6757 = CARTESIAN_POINT ( 'NONE',  ( 13.49926719046979784, 57.43485129297997815, -0.1416316033574115951 ) ) ;
#6758 = CARTESIAN_POINT ( 'NONE',  ( 11.76794919243112325, 67.43000000000000682, 1.441158131103945434E-15 ) ) ;
#6759 = CARTESIAN_POINT ( 'NONE',  ( 3.636496289402157078, 74.03000000000000114, -11.19198476289190936 ) ) ;
#6760 = CARTESIAN_POINT ( 'NONE',  ( -9.831588973340092963, 47.28954498157629871, 9.251600547029006805 ) ) ;
#6761 = AXIS2_PLACEMENT_3D ( 'NONE', #4122, #11996, #9536 ) ;
#6762 = CARTESIAN_POINT ( 'NONE',  ( 0.000000000000000000, 0.000000000000000000, 0.000000000000000000 ) ) ;
#6763 = CARTESIAN_POINT ( 'NONE',  ( -8.000000000000143885, 7.773118517290097174, 17.32050807568870709 ) ) ;
#6764 = CARTESIAN_POINT ( 'NONE',  ( 16.45599557390471546, -100.0000000000000142, 8.218326127789341129 ) ) ;
#6765 = CARTESIAN_POINT ( 'NONE',  ( -4.171729424061791036, 76.53000000000000114, 12.83926296998457239 ) ) ;
#6766 = CARTESIAN_POINT ( 'NONE',  ( -11.37499999999960387, -40.58437499999990905, -4.711679271994910323 ) ) ;
#6767 = CARTESIAN_POINT ( 'NONE',  ( 8.343458848123583849, 6.880000000000006999, -11.48378591275253768 ) ) ;
#6768 = CARTESIAN_POINT ( 'NONE',  ( 13.48854948779883856, 33.44913808748793826, -0.5559301001735216241 ) ) ;
#6769 = CARTESIAN_POINT ( 'NONE',  ( -4.986796838729953940, 73.35992462257202362, -12.54519991607214457 ) ) ;
#6770 = EDGE_LOOP ( 'NONE', ( #15669, #8559, #14163, #12129, #9128, #14435, #8079, #5277, #3911, #485, #8018, #6107, #12810, #5975, #7841, #14389, #6604, #15855, #12000, #2133, #741, #410, #3930, #7665, #8717, #4916, #11764, #6663, #496, #7361, #16908, #5279, #12303, #14758, #2025, #2692, #14222, #14715, #6601 ) ) ;
#6771 = ORIENTED_EDGE ( 'NONE', *, *, #9474, .F. ) ;
#6772 = CARTESIAN_POINT ( 'NONE',  ( -8.291044507619272909E-14, 45.17999999999999972, -13.50000000000000000 ) ) ;
#6773 = EDGE_LOOP ( 'NONE', ( #15808, #11284, #15648, #14847 ) ) ;
#6774 = CARTESIAN_POINT ( 'NONE',  ( -11.37499999999960210, -81.13437499999982094, -4.711679271994911211 ) ) ;
#6775 = AXIS2_PLACEMENT_3D ( 'NONE', #17205, #13314, #941 ) ;
#6776 = CARTESIAN_POINT ( 'NONE',  ( -0.7753613165686097375, 44.65212122024217933, 13.47790793914508001 ) ) ;
#6777 = CARTESIAN_POINT ( 'NONE',  ( 10.92172942406179104, 16.72999999999999332, -7.935100905948385908 ) ) ;
#6778 = EDGE_CURVE ( 'NONE', #15607, #5186, #5433, .T. ) ;
#6779 = CARTESIAN_POINT ( 'NONE',  ( -7.499999999999992895, -22.25853674790686298, 9.367496997597607233 ) ) ;
#6780 = CARTESIAN_POINT ( 'NONE',  ( -8.343458848123576743, 43.47999999999998977, -11.48378591275254301 ) ) ;
#6781 = CARTESIAN_POINT ( 'NONE',  ( 13.50000000000000000, 47.42999999999999972, 1.653273178848926867E-15 ) ) ;
#6782 = CARTESIAN_POINT ( 'NONE',  ( -13.40458808007928049, 70.87413862071015558, -1.602539714754670719 ) ) ;
#6783 = CARTESIAN_POINT ( 'NONE',  ( 7.714727599197340524, -39.57812499999989342, 18.62500000000063949 ) ) ;
#6784 = CARTESIAN_POINT ( 'NONE',  ( -11.80864895165088591, 67.68745830797494989, -6.543130247569663105 ) ) ;
#6785 = CARTESIAN_POINT ( 'NONE',  ( 1.561832610794586740E-12, -30.21249999999990976, -18.62500000000000000 ) ) ;
#6786 = CARTESIAN_POINT ( 'NONE',  ( 11.48581846909945270, 54.69492073424584788, -7.094357488526240374 ) ) ;
#6787 = CARTESIAN_POINT ( 'NONE',  ( 0.000000000000000000, 9.000000000000000000, 0.000000000000000000 ) ) ;
#6788 = CARTESIAN_POINT ( 'NONE',  ( -11.89680182002208042, 64.69398173927839935, -6.380922029939451789 ) ) ;
#6789 = FACE_OUTER_BOUND ( 'NONE', #8103, .T. ) ;
#6790 = CARTESIAN_POINT ( 'NONE',  ( -13.47775970262104295, 34.90311458208528705, -0.7771305193947938283 ) ) ;
#6791 = CARTESIAN_POINT ( 'NONE',  ( 4.171729424061789260, 21.83000000000001606, 12.83926296998457239 ) ) ;
#6792 = VERTEX_POINT ( 'NONE', #2901 ) ;
#6793 = CARTESIAN_POINT ( 'NONE',  ( -11.06327252796750926, 9.630592963500558854E-15, -6.703345338116586838 ) ) ;
#6794 = EDGE_CURVE ( 'NONE', #5870, #10663, #10010, .T. ) ;
#6795 = VECTOR ( 'NONE', #6300, 1000.000000000000000 ) ;
#6796 = CARTESIAN_POINT ( 'NONE',  ( 2.107853069822502790E-14, 31.18000000000000682, -13.50000000000000000 ) ) ;
#6797 = CARTESIAN_POINT ( 'NONE',  ( 4.584035459419017577, 73.01499104528438977, -12.69792770427072348 ) ) ;
#6798 = CARTESIAN_POINT ( 'NONE',  ( -9.520470885617717371, -7.769999999999999574, 6.917026985038133624 ) ) ;
#6799 = DIRECTION ( 'NONE',  ( -0.4999999999999918399, 0.000000000000000000, -0.8660254037844434816 ) ) ;
#6800 = CARTESIAN_POINT ( 'NONE',  ( 2.621994543952811015E-15, -15.82000000000000561, -14.19474002721660355 ) ) ;
#6801 = CARTESIAN_POINT ( 'NONE',  ( -13.39856879038537585, 52.87025179575815770, -1.714939770267754460 ) ) ;
#6802 = CARTESIAN_POINT ( 'NONE',  ( -11.76794919243112325, 50.77999999999998693, -3.823638476888998827 ) ) ;
#6803 = CARTESIAN_POINT ( 'NONE',  ( -10.92172942406179104, 64.23000000000000398, 7.935100905948387684 ) ) ;
#6804 = CARTESIAN_POINT ( 'NONE',  ( 3.659205458685654833, 50.81139327735426292, 12.99542509430799875 ) ) ;
#6805 = CARTESIAN_POINT ( 'NONE',  ( -5.561034285559797397, 37.38178090531955178, -12.30142152455749915 ) ) ;
#6806 = CARTESIAN_POINT ( 'NONE',  ( 4.138376238514326566, 35.82879951124870388, 12.85007333697660492 ) ) ;
#6807 = CARTESIAN_POINT ( 'NONE',  ( 7.714727599197340524, -37.42812499999993037, 18.62500000000063949 ) ) ;
#6808 = CARTESIAN_POINT ( 'NONE',  ( -9.503523212203964121, 74.30641799480795839, 9.597461011868634984 ) ) ;
#6809 =( BOUNDED_CURVE ( )  B_SPLINE_CURVE ( 2, ( #4081, #9496, #14843, #2737, #12141, #9512, #5528, #11001, #7115, #5436, #10823, #7032, #5707 ),
 .UNSPECIFIED., .F., .F. ) 
 B_SPLINE_CURVE_WITH_KNOTS ( ( 3, 2, 2, 2, 2, 2, 3 ),
 ( 0.1805555555555555525, 0.1833333333333333204, 0.1888888888888888840, 0.1944444444444444475, 0.2000000000000000111, 0.2055555555555555469, 0.2083333333333333148 ),
 .UNSPECIFIED. ) 
 CURVE ( )  GEOMETRIC_REPRESENTATION_ITEM ( )  RATIONAL_B_SPLINE_CURVE ( ( 0.9755282581475768211, 0.9755282581475768211, 1.000000000000000000, 0.9510565162951535312, 1.000000000000000000, 0.9510565162951535312, 1.000000000000000000, 0.9510565162951535312, 1.000000000000000000, 0.9510565162951535312, 1.000000000000000000, 0.9755282581475768211, 0.9755282581475765991 ) ) 
 REPRESENTATION_ITEM ( '' )  );
#6810 = CARTESIAN_POINT ( 'NONE',  ( -10.79961255144821841, 76.62273742997086856, -8.101642849603434726 ) ) ;
#6811 = CARTESIAN_POINT ( 'NONE',  ( -6.743467333083651205, 79.42893378531856285, -11.69562671412998611 ) ) ;
#6812 = CARTESIAN_POINT ( 'NONE',  ( -3.636496289402152637, 9.330000000000005400, -11.19198476289190936 ) ) ;
#6813 = CARTESIAN_POINT ( 'NONE',  ( -9.639429313059489246, 80.92999999999997840, 7.743379967843619482 ) ) ;
#6814 = FACE_OUTER_BOUND ( 'NONE', #11965, .T. ) ;
#6815 = CARTESIAN_POINT ( 'NONE',  ( -7.272992578804310604, 1.379999999999991456, 10.01041549318726709 ) ) ;
#6816 = CARTESIAN_POINT ( 'NONE',  ( 9.520470885617715595, 52.12999999999999545, 6.917026985038134512 ) ) ;
#6817 = CARTESIAN_POINT ( 'NONE',  ( -11.37500000000000000, -41.62499999999990052, -9.545674412382054647E-13 ) ) ;
#6818 = CARTESIAN_POINT ( 'NONE',  ( 18.62499999999934630, -32.25937499999992042, 7.714727599200467800 ) ) ;
#6819 = CARTESIAN_POINT ( 'NONE',  ( -8.343458848123576743, -7.520000000000004015, -11.48378591275254301 ) ) ;
#6820 = CARTESIAN_POINT ( 'NONE',  ( -12.51283734680061421, 40.74519236365699015, -5.085795480612188335 ) ) ;
#6821 = DIRECTION ( 'NONE',  ( 0.000000000000000000, 1.000000000000000000, 0.000000000000000000 ) ) ;
#6822 = CARTESIAN_POINT ( 'NONE',  ( 12.07265237676784153, 75.20733480710443075, 6.044380633809719683 ) ) ;
#6823 = CARTESIAN_POINT ( 'NONE',  ( 16.37694731117742464, 1.089405092048505075E-13, -8.432838350389969762 ) ) ;
#6824 = CARTESIAN_POINT ( 'NONE',  ( -7.000496543013151829, 41.42031948789649221, 11.54310368834964251 ) ) ;
#6825 = CARTESIAN_POINT ( 'NONE',  ( -7.758731431966043424, 58.47177289251840904, -11.07319905588548536 ) ) ;
#6826 = CARTESIAN_POINT ( 'NONE',  ( 0.6222550924804421957, 44.70229475783964546, 13.50000000005490719 ) ) ;
#6827 = CARTESIAN_POINT ( 'NONE',  ( -9.999999999999776179, 7.983052681820796970, -15.32050807568890427 ) ) ;
#6828 = DIRECTION ( 'NONE',  ( -1.000000000000000000, -0.000000000000000000, -0.000000000000000000 ) ) ;
#6829 = EDGE_CURVE ( 'NONE', #225, #10490, #14880, .T. ) ;
#6830 = DIRECTION ( 'NONE',  ( -0.000000000000000000, 1.000000000000000000, -0.000000000000000000 ) ) ;
#6831 = CARTESIAN_POINT ( 'NONE',  ( -13.43717355439436645, 49.88445258502782309, -1.313953709901692468 ) ) ;
#6832 = VECTOR ( 'NONE', #2197, 1000.000000000000000 ) ;
#6833 = CARTESIAN_POINT ( 'NONE',  ( 13.37133377648401833, 63.49501688011058320, -1.859467621360270995 ) ) ;
#6834 = CARTESIAN_POINT ( 'NONE',  ( 12.29909249565109874, 42.22626233038081978, 5.566308865609547851 ) ) ;
#6835 = CARTESIAN_POINT ( 'NONE',  ( -18.46710335681943960, 7.924935997292880785, -1.296119813004219079 ) ) ;
#6836 = VERTEX_POINT ( 'NONE', #1821 ) ;
#6837 = CYLINDRICAL_SURFACE ( 'NONE', #16997, 1.999999999999998224 ) ;
#6838 = DIRECTION ( 'NONE',  ( 1.000000000000000000, 0.000000000000000000, 0.000000000000000000 ) ) ;
#6839 = CARTESIAN_POINT ( 'NONE',  ( 13.49999999999999822, 15.28000000000000469, 4.386415899144237684 ) ) ;
#6840 = EDGE_LOOP ( 'NONE', ( #1015, #3183, #2106, #10298 ) ) ;
#6841 = CARTESIAN_POINT ( 'NONE',  ( -8.711585423346765111, 43.51545218957856775, -10.31301875482525432 ) ) ;
#6842 = CARTESIAN_POINT ( 'NONE',  ( -7.499999999999997335, 107.2276959944579886, 6.931232109908918027 ) ) ;
#6843 = CARTESIAN_POINT ( 'NONE',  ( 10.55993636637368915, 60.75057338229004245, -8.410584490247227762 ) ) ;
#6844 = CARTESIAN_POINT ( 'NONE',  ( 4.171729424061791924, 14.03000000000001535, -12.83926296998457239 ) ) ;
#6845 = CARTESIAN_POINT ( 'NONE',  ( 9.788623329136655116, 72.06825703125207383, 9.296935394730732938 ) ) ;
#6846 = CARTESIAN_POINT ( 'NONE',  ( 12.07674395289608427, 66.65302372406806342, -6.058184999537175486 ) ) ;
#6847 = CARTESIAN_POINT ( 'NONE',  ( 5.007094059867902125, 56.86068527283545393, 12.53717015245978139 ) ) ;
#6848 = CARTESIAN_POINT ( 'NONE',  ( 11.76794919243112680, 73.58000000000001251, -3.823638476888993942 ) ) ;
#6849 = CARTESIAN_POINT ( 'NONE',  ( 11.76794919243112680, 70.58000000000001251, -3.823638476888993942 ) ) ;
#6850 = VECTOR ( 'NONE', #11262, 1000.000000000000227 ) ;
#6851 = CARTESIAN_POINT ( 'NONE',  ( -11.31822579835496434, 47.20583829161283518, 7.358718820380858006 ) ) ;
#6852 = CARTESIAN_POINT ( 'NONE',  ( 5.395622418065101122, 45.98446605595357539, -12.37542908175213796 ) ) ;
#6853 = CARTESIAN_POINT ( 'NONE',  ( 1.900613283894444283, 7.890856018535865601, 12.00000000000006040 ) ) ;
#6854 = CARTESIAN_POINT ( 'NONE',  ( 8.006520823759419869, -99.99999999999997158, 15.10378497192285785 ) ) ;
#6855 = CARTESIAN_POINT ( 'NONE',  ( -2.328902225919929236, 56.59619329505072471, 13.29813340977210778 ) ) ;
#6856 = CARTESIAN_POINT ( 'NONE',  ( -8.043339635996302306, -89.49374999999979252, -8.043339635997654113 ) ) ;
#6857 = DIRECTION ( 'NONE',  ( -1.000000000000000000, 0.000000000000000000, 0.000000000000000000 ) ) ;
#6858 = CARTESIAN_POINT ( 'NONE',  ( 11.94107144633697892, 33.66270217958954447, -6.298310357517227231 ) ) ;
#6859 = CARTESIAN_POINT ( 'NONE',  ( -9.645889337515697548, 73.56097694870044279, -9.444937062324340715 ) ) ;
#6860 = LINE ( 'NONE', #5801, #14230 ) ;
#6861 = CARTESIAN_POINT ( 'NONE',  ( -11.76794919243112325, 24.93000000000000682, -2.602085213965210642E-15 ) ) ;
#6862 = EDGE_LOOP ( 'NONE', ( #3561, #16485, #5075, #9852 ) ) ;
#6863 = CARTESIAN_POINT ( 'NONE',  ( -8.343458848123578520, 42.47999999999999687, -11.48378591275254124 ) ) ;
#6864 = ORIENTED_EDGE ( 'NONE', *, *, #8742, .F. ) ;
#6865 = VECTOR ( 'NONE', #2010, 1000.000000000000000 ) ;
#6866 = CARTESIAN_POINT ( 'NONE',  ( -13.48209528736951768, 40.90592558830504544, -0.6972090822305906377 ) ) ;
#6867 = CARTESIAN_POINT ( 'NONE',  ( 9.520470885617715595, -12.86999999999999922, 6.917026985038135400 ) ) ;
#6868 = CARTESIAN_POINT ( 'NONE',  ( -4.711679271994915652, -85.29687499999980105, 11.37499999999960210 ) ) ;
#6869 = CARTESIAN_POINT ( 'NONE',  ( -11.51090208011366478, 44.19368821836776817, 7.064733831953415866 ) ) ;
#6870 = CARTESIAN_POINT ( 'NONE',  ( -7.499999999999996447, -21.99999999999990052, 9.367496997597656971 ) ) ;
#6871 = CARTESIAN_POINT ( 'NONE',  ( 10.92172942406178926, 42.13000000000000256, 7.935100905948387684 ) ) ;
#6872 = CARTESIAN_POINT ( 'NONE',  ( -13.49999999999999822, 48.77999999999998693, -4.386415899144240349 ) ) ;
#6873 = CARTESIAN_POINT ( 'NONE',  ( -13.49787322744430362, 70.92177515562346457, -0.2398385319287087425 ) ) ;
#6874 = AXIS2_PLACEMENT_3D ( 'NONE', #608, #11572, #13937 ) ;
#6875 = CARTESIAN_POINT ( 'NONE',  ( 7.714727599197340524, -22.92812499999992326, 18.62500000000063949 ) ) ;
#6876 = ADVANCED_FACE ( 'NONE', ( #3150 ), #2882, .F. ) ;
#6877 = CARTESIAN_POINT ( 'NONE',  ( -2.941772209709978103, 67.28577460440457969, -13.17558263144108466 ) ) ;
#6878 = CARTESIAN_POINT ( 'NONE',  ( 18.62499999999934630, -98.85937499999975842, 7.714727599200467800 ) ) ;
#6879 = B_SPLINE_CURVE_WITH_KNOTS ( 'NONE', 3,
 ( #10983, #10893, #13616, #16353, #9669, #16443, #8428, #15019, #2911, #7013, #13781, #1680, #7096, #366, #5771, #11155, #16531, #4438, #14048, #538, #16620, #5863, #4698, #15280, #8603, #4524, #15540, #7265, #1770, #626, #9931, #15366, #12649, #12738, #4870, #12567, #3363, #3181, #453, #7359, #1936, #8689, #11242, #11591, #10273, #795, #14219, #16792, #12827, #11328, #13955, #1852, #6037, #5948, #15624, #16706, #4611, #10018, #12911, #3272, #11420, #15454, #8867, #10103, #8779, #7179, #14135, #2023, #7448, #2104, #714, #6125, #11504, #16880, #4785, #10186, #16967, #3452, #7531, #6205, #3532, #13868, #4903, #14335, #574, #12858, #7478, #4816, #6235, #8895, #5981, #658, #12684, #3481, #4731, #15655, #2136, #1967, #2224, #10302, #6067, #11363, #15313, #10050, #10217, #12598, #15400, #11450, #3308, #13988, #488, #16824, #14250, #11274, #8809, #4558, #9963, #5894, #7562, #10132, #16650, #15486, #3396, #8637, #1884, #12940, #14166, #7299, #16738, #8721, #3565, #748, #8979, #6322, #10646, #9417, #4001, #1256, #13029, #4990, #2480, #11797, #10564, #912, #11708, #13367, #14422, #9247, #2310, #17085, #7830, #17174, #10392, #16009, #14765, #7653, #5084, #6587, #15746, #3657, #9069, #11885, #7739 ),
 .UNSPECIFIED., .F., .F.,
 ( 4, 2, 2, 2, 2, 1, 1, 1, 2, 2, 2, 2, 1, 1, 2, 2, 1, 2, 2, 2, 2, 1, 1, 2, 2, 2, 2, 1, 2, 2, 1, 1, 2, 2, 1, 1, 1, 2, 2, 2, 2, 2, 1, 1, 1, 2, 2, 1, 2, 2, 2, 2, 1, 2, 2, 1, 1, 2, 2, 2, 2, 2, 2, 2, 2, 2, 1, 1, 2, 2, 1, 2, 2, 1, 2, 2, 2, 2, 1, 2, 2, 1, 2, 2, 2, 2, 1, 1, 1, 1, 1, 1, 2, 2, 2, 2, 2, 4 ),
 ( 0.6225616101408076863, 0.6262466207516538264, 0.6267072470780096216, 0.6268224036595985149, 0.6268367982322970988, 0.6268511928049957938, 0.6268799819503929616, 0.6269375602411875192, 0.6271678734043656389, 0.6280891260570777845, 0.6285497523834339129, 0.6287800655466120325, 0.6288952221282010369, 0.6289528004189955945, 0.6289671949916941784, 0.6289815895643928734, 0.6290103787097900412, 0.6299316313625022978, 0.6308528840152144435, 0.6310831971783924521, 0.6311119863237897309, 0.6311407754691870098, 0.6311983537599814564, 0.6313135103415704608, 0.6317741366679265891, 0.6326953893206387347, 0.6331560156469947520, 0.6332135939377891987, 0.6332279885104878936, 0.6332423830831864775, 0.6332711722285837563, 0.6333863288101727607, 0.6336166419733507693, 0.6345378946260628039, 0.6349985209524187102, 0.6352288341155967188, 0.6353439906971857232, 0.6353727798425830020, 0.6354015689879802808, 0.6354591472787747275, 0.6363803999314867621, 0.6373016525841987967, 0.6374168091657878010, 0.6374743874565823587, 0.6375031766019796375, 0.6375103738883288740, 0.6375175711746782214, 0.6375319657473768054, 0.6377622789105548140, 0.6382229052369109423, 0.6391441578896229769, 0.6396047842159791053, 0.6396335733613763841, 0.6396479679340749680, 0.6396551652204243155, 0.6396623625067735519, 0.6397199407975681096, 0.6398350973791571139, 0.6400654105423351226, 0.6409866631950471572, 0.6419079158477593028, 0.6421382290109373114, 0.6422533855925263158, 0.6423685421741153201, 0.6428291685004713374, 0.6432897948268273547, 0.6433473731176219124, 0.6433761622630190802, 0.6433905568357177751, 0.6434049514084163590, 0.6435201079900053633, 0.6437504211531833720, 0.6442110474795395003, 0.6444413606427175090, 0.6445565172243065133, 0.6446716738058955176, 0.6465141791113196978, 0.6469748054376757151, 0.6470899620192647195, 0.6471475403100592771, 0.6471763294554564450, 0.6472051186008537238, 0.6474354317640317324, 0.6483566844167438781, 0.6483854735621411569, 0.6484142627075384357, 0.6484718409983329934, 0.6485869975799219977, 0.6488173107431000064, 0.6492779370694561347, 0.6495082502326341434, 0.6496234068142231477, 0.6496521959596204265, 0.6496809851050177054, 0.6497385633958121520, 0.6501991897221682803, 0.6511204423748804260, 0.6520416950275925716 ),
 .UNSPECIFIED. ) ;
#6880 = CARTESIAN_POINT ( 'NONE',  ( 12.86363371229788477, 54.28279489801139590, 4.098915096101688249 ) ) ;
#6881 = CARTESIAN_POINT ( 'NONE',  ( -13.09608275284783296, 64.81328617085095800, -3.281779600780347916 ) ) ;
#6882 = ORIENTED_EDGE ( 'NONE', *, *, #3504, .T. ) ;
#6883 = LINE ( 'NONE', #12255, #9786 ) ;
#6884 = CARTESIAN_POINT ( 'NONE',  ( -13.21814477936476706, 34.83246129253718948, -2.760861401621048206 ) ) ;
#6885 = ORIENTED_EDGE ( 'NONE', *, *, #4165, .T. ) ;
#6886 = CARTESIAN_POINT ( 'NONE',  ( 12.83398559654505533, 78.27937745505627731, 4.188225396753645136 ) ) ;
#6887 = CARTESIAN_POINT ( 'NONE',  ( 25.42428528562856727, 5.918584287042170544, -5.441113646577394825 ) ) ;
#6888 = CARTESIAN_POINT ( 'NONE',  ( -5.362442804292004261, 31.37413780983099798, -12.38972965817070993 ) ) ;
#6889 = CARTESIAN_POINT ( 'NONE',  ( 8.302743629395873626, 72.86345579277633533, -10.64494644169182003 ) ) ;
#6890 = CARTESIAN_POINT ( 'NONE',  ( 2.612430725649731666, 59.77398820739121987, 13.24767911791428432 ) ) ;
#6891 = CARTESIAN_POINT ( 'NONE',  ( -13.49999999999999822, -18.22000000000000242, -4.386415899144240349 ) ) ;
#6892 = CARTESIAN_POINT ( 'NONE',  ( 8.343458848123583849, 72.88000000000000966, -11.48378591275253768 ) ) ;
#6893 = CARTESIAN_POINT ( 'NONE',  ( -11.56380442966215050, 52.67022467909172434, -6.968482334245324594 ) ) ;
#6894 = CARTESIAN_POINT ( 'NONE',  ( 9.520470885617717371, 52.72999999999999687, -6.917026985038131848 ) ) ;
#6895 = CARTESIAN_POINT ( 'NONE',  ( 13.49999999999999822, 71.28000000000000114, 4.386415899144237684 ) ) ;
#6896 = CYLINDRICAL_SURFACE ( 'NONE', #1079, 26.00000000000000355 ) ;
#6897 = CARTESIAN_POINT ( 'NONE',  ( 11.67283399857811155, 69.68278107398599275, -6.798365021777054373 ) ) ;
#6898 = CARTESIAN_POINT ( 'NONE',  ( -12.91217337725079517, 37.78870154777813894, -3.941070675155305292 ) ) ;
#6899 = ADVANCED_FACE ( 'NONE', ( #9726 ), #6896, .T. ) ;
#6900 = CARTESIAN_POINT ( 'NONE',  ( 5.972235571882229976, 35.89753408868532603, 12.11506502541500296 ) ) ;
#6901 = CARTESIAN_POINT ( 'NONE',  ( 18.62500000000064659, -41.59062499999991758, -7.714727599197336083 ) ) ;
#6902 = CARTESIAN_POINT ( 'NONE',  ( -12.28445251099280355, 74.13502960058168867, 5.602360786159263917 ) ) ;
#6903 = CARTESIAN_POINT ( 'NONE',  ( -13.49315368495419065, 76.90577415051416210, -0.6964660162547660072 ) ) ;
#6904 = CARTESIAN_POINT ( 'NONE',  ( -4.960630769662208728, 79.35887515246722046, -12.55750558105645354 ) ) ;
#6905 = CARTESIAN_POINT ( 'NONE',  ( -3.565931047812489929, 80.93000000000003524, 12.36697741789239480 ) ) ;
#6906 = CARTESIAN_POINT ( 'NONE',  ( -2.138189944381279073, 7.256881422320270225, -13.49999999999998579 ) ) ;
#6907 = CARTESIAN_POINT ( 'NONE',  ( -7.272992578804310604, -1.620000000000001217, 10.01041549318726709 ) ) ;
#6908 = CARTESIAN_POINT ( 'NONE',  ( -11.76794919243112325, 45.08000000000000540, 3.823638476888994830 ) ) ;
#6909 = CARTESIAN_POINT ( 'NONE',  ( 8.343458848123583849, -17.12000000000000099, -11.48378591275253768 ) ) ;
#6910 = CARTESIAN_POINT ( 'NONE',  ( -9.982813566452611198, 40.57839600760536314, -9.089889854899778854 ) ) ;
#6911 = DIRECTION ( 'NONE',  ( 1.000000000000000000, 0.000000000000000000, 0.000000000000000000 ) ) ;
#6912 = CARTESIAN_POINT ( 'NONE',  ( 13.06332958711276859, 75.55131820085146899, -3.405797684387579238 ) ) ;
#6913 = CARTESIAN_POINT ( 'NONE',  ( 3.077395063295970790, 9.636628673746354086E-15, -14.72315406558967688 ) ) ;
#6914 = CARTESIAN_POINT ( 'NONE',  ( -9.593668878646951725, 41.30170092094060408, 9.501538401032471270 ) ) ;
#6915 = CARTESIAN_POINT ( 'NONE',  ( -4.434027931263471167, 58.33950993581493094, -12.75153076942259034 ) ) ;
#6916 =( BOUNDED_CURVE ( )  B_SPLINE_CURVE ( 2, ( #7862, #2174, #11833, #7600, #15608, #17035, #5027, #10513, #15875, #11658, #2431, #5208, #4940 ),
 .UNSPECIFIED., .F., .F. ) 
 B_SPLINE_CURVE_WITH_KNOTS ( ( 3, 2, 2, 2, 2, 2, 3 ),
 ( 0.4386822870511441486, 0.4415124951778801599, 0.4471729117827247801, 0.4528333283875693449, 0.4584937449924140207, 0.4641541615972585855, 0.4669843698996809511 ),
 .UNSPECIFIED. ) 
 CURVE ( )  GEOMETRIC_REPRESENTATION_ITEM ( )  RATIONAL_B_SPLINE_CURVE ( ( 0.9755282581475768211, 0.9755282596666697836, 1.000000000000000000, 0.9510565162951535312, 1.000000000000000000, 0.9510565162951535312, 1.000000000000000000, 0.9510565162951535312, 1.000000000000000000, 0.9510565162951535312, 1.000000000000000000, 0.9755282581475765991, 0.9755282581475768211 ) ) 
 REPRESENTATION_ITEM ( '' )  );
#6917 = CARTESIAN_POINT ( 'NONE',  ( 2.904295422893758527, 44.78442768824688613, 13.18389593751376410 ) ) ;
#6918 = ADVANCED_FACE ( 'NONE', ( #3240 ), #16503, .F. ) ;
#6919 = LINE ( 'NONE', #17332, #7244 ) ;
#6920 = FACE_OUTER_BOUND ( 'NONE', #11163, .T. ) ;
#6921 = CARTESIAN_POINT ( 'NONE',  ( -15.58845726811976995, 7.773118517290098062, -11.00000000000018119 ) ) ;
#6922 = CARTESIAN_POINT ( 'NONE',  ( -13.47928820673223527, 49.90421348230867693, -0.7476691059968105790 ) ) ;
#6923 = CARTESIAN_POINT ( 'NONE',  ( 12.10713279764149775, 63.65069317145754724, -6.000162191947801205 ) ) ;
#6924 = CARTESIAN_POINT ( 'NONE',  ( 12.35813771356544422, 42.23148437247772335, 5.433829964281000180 ) ) ;
#6925 = CARTESIAN_POINT ( 'NONE',  ( 6.741586065090841018, 38.92882405296342085, 11.69831271653080584 ) ) ;
#6926 = VERTEX_POINT ( 'NONE', #337 ) ;
#6927 = CARTESIAN_POINT ( 'NONE',  ( -9.552639591052204498E-13, -12.48749999999997051, 11.37500000000000000 ) ) ;
#6928 = CARTESIAN_POINT ( 'NONE',  ( -13.49999999999999822, 14.07999999999999652, 4.386415899144235908 ) ) ;
#6929 = ORIENTED_EDGE ( 'NONE', *, *, #7092, .F. ) ;
#6930 = CARTESIAN_POINT ( 'NONE',  ( -9.339320245421074418, 43.54553106418224928, -9.750580036500519299 ) ) ;
#6931 = CARTESIAN_POINT ( 'NONE',  ( -7.499999999999999112, 103.4461236652718696, 9.346045933502388436 ) ) ;
#6932 = CARTESIAN_POINT ( 'NONE',  ( 12.04411969963108220, 60.65532207379116159, -6.117687879866321232 ) ) ;
#6933 = PRODUCT_DEFINITION_SHAPE ( 'NONE', 'NONE',  #48 ) ;
#6934 = CARTESIAN_POINT ( 'NONE',  ( 8.343458848123578520, 12.98000000000000220, 11.48378591275254124 ) ) ;
#6935 = CARTESIAN_POINT ( 'NONE',  ( 0.000000000000000000, 102.9300000000000068, 0.000000000000000000 ) ) ;
#6936 = CARTESIAN_POINT ( 'NONE',  ( 11.58799853746032227, 66.68808562819272368, -6.925914820338668676 ) ) ;
#6937 = CARTESIAN_POINT ( 'NONE',  ( 2.660236471785744961, 56.77572940497019260, 13.23661507586563779 ) ) ;
#6938 = CARTESIAN_POINT ( 'NONE',  ( 9.520470885617717371, 55.73000000000000398, -6.917026985038131848 ) ) ;
#6939 = CARTESIAN_POINT ( 'NONE',  ( 3.636496289402154414, 66.82999999999999829, 11.19198476289190936 ) ) ;
#6940 = CARTESIAN_POINT ( 'NONE',  ( -12.01013503625162215, 47.15762422974843560, 6.171082197149440951 ) ) ;
#6941 = CARTESIAN_POINT ( 'NONE',  ( 5.441113646577305119, 0.000000000000000000, 25.42428528562857792 ) ) ;
#6942 = CARTESIAN_POINT ( 'NONE',  ( -2.838270712586780596E-14, 67.18000000000000682, -13.50000000000000178 ) ) ;
#6943 = DIRECTION ( 'NONE',  ( 0.000000000000000000, 0.000000000000000000, 1.000000000000000000 ) ) ;
#6944 = CARTESIAN_POINT ( 'NONE',  ( -8.547853120570341190, 56.35218660269319457, 10.44914891313210070 ) ) ;
#6945 = CARTESIAN_POINT ( 'NONE',  ( -11.37499999999960387, -57.23437499999987921, -4.711679271994910323 ) ) ;
#6946 = CARTESIAN_POINT ( 'NONE',  ( -9.999999999999776179, 0.000000000000000000, -17.32050807568890605 ) ) ;
#6947 = CARTESIAN_POINT ( 'NONE',  ( 12.03035526396323363, 33.65579982725444097, -6.125565056414373544 ) ) ;
#6948 = B_SPLINE_CURVE_WITH_KNOTS ( 'NONE', 3,
 ( #687, #14362, #14279, #4674, #3592, #10165, #10079, #11481, #14451, #1029, #3425, #10331, #15430, #15685, #11734, #2338, #7590, #6180, #17112, #11394, #11566, #3339, #6262, #7422, #8754, #16940, #15774, #17026, #8840, #14197, #10416, #9098, #3507, #10246, #1995, #4842, #4930, #16766, #15599, #16856, #4759, #2250, #2079, #7504, #8920, #2165, #12969, #16208, #1202, #9271, #2684, #17287, #5199, #7852, #14707, #11908, #12163, #17203, #5458, #6530, #14623, #10671, #14877, #5111, #2419, #15951, #3943, #54, #15866, #3773, #17455, #16119, #14534, #5289, #6696, #16035, #1116, #13311, #9358, #10841, #13393, #11993, #11823, #6440, #6613, #5369, #2509, #13227, #8204, #4119, #10589, #9533, #13566, #3857, #10756, #10504, #4030, #8115, #2773, #2596, #17375, #9186, #7939, #8025, #1282, #12076, #9444, #14792, #13481, #1369, #6784, #234, #5640, #15234, #3130, #11108, #317, #145, #13736, #7134, #9969, #493, #14972, #12342, #1721, #11022, #4296, #5900, #16394, #9709, #11279, #1634, #15053, #8555, #2953, #8381, #2862, #9796, #6964, #7217, #12250, #11197, #8642, #8470, #5726, #15317, #5551, #8294, #7051, #16481, #12604, #10934, #16301, #12522, #16573, #9621, #4385, #406, #15142, #13651, #12431, #1803, #3039, #16656, #13820, #6877, #1457, #5813, #4478, #9884, #1545, #3220, #4563, #13908, #4208, #10398, #11456, #10310, #7484, #3665, #6243, #1890, #6076, #16832, #2147, #15755, #13995, #17004 ),
 .UNSPECIFIED., .F., .F.,
 ( 4, 2, 1, 1, 2, 2, 1, 2, 2, 2, 1, 1, 2, 2, 2, 2, 2, 2, 2, 2, 1, 1, 1, 1, 1, 2, 2, 2, 1, 2, 2, 1, 1, 1, 2, 2, 2, 2, 2, 1, 1, 2, 2, 2, 2, 2, 2, 1, 1, 2, 1, 1, 2, 2, 2, 2, 1, 1, 1, 2, 2, 2, 2, 2, 2, 2, 2, 2, 2, 1, 1, 1, 2, 1, 2, 2, 1, 1, 2, 1, 2, 2, 1, 1, 2, 2, 2, 2, 1, 2, 2, 2, 2, 2, 1, 1, 2, 2, 1, 1, 2, 2, 1, 1, 1, 2, 2, 2, 2, 1, 2, 2, 1, 2, 4 ),
 ( 0.2402135124365048502, 0.2406730745069247945, 0.2409028555421347806, 0.2410177460597397736, 0.2410464686891410080, 0.2410751913185422701, 0.2411326365773447389, 0.2420517607181846276, 0.2429708848590244885, 0.2432006658942344468, 0.2432581111530369433, 0.2432868337824382055, 0.2433011950971388226, 0.2433155564118394398, 0.2434304469294444606, 0.2438900089998645160, 0.2448091331407046545, 0.2457282572815447930, 0.2466473814223849315, 0.2466617427370855764, 0.2466761040517861936, 0.2467048266811874557, 0.2467622719399899522, 0.2468771624575949730, 0.2471069434928050146, 0.2475665055632250700, 0.2494047538449053469, 0.2498643159153254301, 0.2499792064329304508, 0.2499935677476310680, 0.2500007484049813766, 0.2500079290623317130, 0.2500366516917329474, 0.2500940969505354716, 0.2503238779857455132, 0.2512430021265857349, 0.2517025641970058181, 0.2519323452322158596, 0.2519610678616171495, 0.2519897904910183839, 0.2520472357498209082, 0.2521621262674259567, 0.2530812504082661785, 0.2535408124786862616, 0.2537705935138963587, 0.2538854840315013517, 0.2539142066609026416, 0.2539429292903038760, 0.2540003745491064002, 0.2544599366195265389, 0.2546897176547365804, 0.2548046081723416290, 0.2548620534311440977, 0.2549194986899466220, 0.2558386228307868437, 0.2558673454601880781, 0.2558960680895893680, 0.2559535133483918923, 0.2560684038659968853, 0.2562981849012069269, 0.2567577469716270100, 0.2576768711124672318, 0.2577917616300722248, 0.2579066521476772733, 0.2581364331828873149, 0.2585959952533073980, 0.2595151193941475642, 0.2597449004293576058, 0.2597736230587588957, 0.2598023456881601301, 0.2598597909469626543, 0.2599746814645676474, 0.2604342435349877305, 0.2606640245701977721, 0.2607214698290002963, 0.2607501924584015307, 0.2607789150878028206, 0.2608938056054078136, 0.2613533676758278412, 0.2615831487110378828, 0.2616980392286428758, 0.2617267618580441657, 0.2617554844874454001, 0.2618129297462479244, 0.2622724918166679520, 0.2631916159575080072, 0.2636511780279280348, 0.2637660685455330833, 0.2638809590631380764, 0.2641107400983480624, 0.2650298642391881176, 0.2654894263096081453, 0.2656043168272131938, 0.2656330394566144282, 0.2656617620860157181, 0.2657192073448181868, 0.2659489883800282284, 0.2668681125208683391, 0.2673276745912884222, 0.2675574556264984638, 0.2675718169411990810, 0.2675789975985494173, 0.2675861782558996982, 0.2676149008853009881, 0.2676723461441035123, 0.2677872366617085609, 0.2687063608025491157, 0.2691659228729693654, 0.2693957039081795179, 0.2695105944257845665, 0.2695249557404851837, 0.2695321363978355200, 0.2695393170551858009, 0.2695680396845870908, 0.2696254849433896150 ),
 .UNSPECIFIED. ) ;
#6949 = CARTESIAN_POINT ( 'NONE',  ( -8.397663224344118049, 9.999999999999998224, 9.034341791799572974 ) ) ;
#6950 = CARTESIAN_POINT ( 'NONE',  ( -8.673064033300265763, 8.051595442100884625, -15.81825948347707822 ) ) ;
#6951 = CARTESIAN_POINT ( 'NONE',  ( -9.520470885617715595, 24.63000000000001322, -6.917026985038136289 ) ) ;
#6952 = ORIENTED_EDGE ( 'NONE', *, *, #13007, .T. ) ;
#6953 = CARTESIAN_POINT ( 'NONE',  ( -1.732050807568877859, 0.000000000000000000, -18.99999999999999645 ) ) ;
#6954 = AXIS2_PLACEMENT_3D ( 'NONE', #15990, #3894, #15637 ) ;
#6955 = ORIENTED_EDGE ( 'NONE', *, *, #2057, .F. ) ;
#6956 = CARTESIAN_POINT ( 'NONE',  ( -13.16986379959834252, -46.79374999999990337, -13.16986379960055409 ) ) ;
#6957 = CARTESIAN_POINT ( 'NONE',  ( -13.46697175398167978, 43.89732407946095805, -0.9441447902741053610 ) ) ;
#6958 = CARTESIAN_POINT ( 'NONE',  ( -8.110285629053095136, 7.924527542031521321, 16.64312382832866888 ) ) ;
#6959 = CARTESIAN_POINT ( 'NONE',  ( 8.343458848123583849, 30.87999999999999901, -11.48378591275253768 ) ) ;
#6960 = CARTESIAN_POINT ( 'NONE',  ( -13.10414842226016496, 71.04706212969732348, 3.294509102343420093 ) ) ;
#6961 = PRESENTATION_LAYER_ASSIGNMENT (  '', '', ( #12602 ) ) ;
#6962 = B_SPLINE_CURVE_WITH_KNOTS ( 'NONE', 3,
 ( #14921, #16076, #12202, #14748, #4158, #13686, #2814, #12032, #17411, #5326, #7004, #4, #3983, #10796, #10973, #16434, #95, #187, #6736, #8419, #6824, #5593, #6650, #5409, #14831, #10710, #1500, #9398, #16341, #16160, #13605, #5500, #9571, #2637, #8068, #10883, #15090, #1320, #6914, #13432, #16253, #12291, #1586, #4249, #12115, #4070, #9485, #12380, #2725, #9659, #8153, #13518, #1409, #2900, #8331, #271, #2989, #1238, #5680, #11060, #4336, #9745, #17192, #6606, #5102, #5191, #17366, #5280, #13472, #3934, #9436, #14785, #8107, #1358, #11013, #43, #16564, #15225, #2943, #310, #5540, #1797, #7209, #14962, #5449, #16384, #16197, #6866, #4110, #10924, #12242, #2852, #4200, #8286, #9611, #226, #7296, #12681, #571, #5978, #11360, #16735, #8240, #10789, #4986, #5405, #2306, #6820, #2720, #12109, #12197, #6318, #857, #5588, #16336, #17081, #15742, #10388, #3653, #9391, #9065, #14418, #907, #4153, #13110, #2632, #7734, #16247, #16155, #9653, #14915, #14742, #15003, #6910, #4064, #10876, #7649, #13025, #17170, #90, #11704, #997, #6410, #9480, #11793, #8063, #5080, #14826, #10475, #15835, #13512, #3740, #1404, #5495, #9565, #12286, #13065, #9014, #12979, #15696, #3435, #6272, #14372, #12896, #5029, #3517, #2349, #11491, #6450, #2089, #10175, #783, #1039, #6190, #7516, #11834, #10256, #11577, #11746, #16952, #15788, #2007, #10429 ),
 .UNSPECIFIED., .F., .F.,
 ( 4, 2, 2, 1, 2, 2, 1, 2, 2, 2, 2, 2, 1, 1, 2, 2, 1, 1, 1, 2, 2, 1, 1, 2, 2, 2, 2, 2, 1, 1, 1, 2, 2, 2, 1, 1, 2, 2, 1, 2, 2, 2, 2, 1, 2, 2, 1, 2, 2, 2, 1, 1, 2, 2, 2, 1, 1, 2, 2, 2, 2, 2, 2, 2, 2, 2, 2, 2, 1, 1, 1, 1, 2, 2, 1, 1, 1, 2, 2, 1, 2, 2, 2, 2, 1, 1, 2, 2, 2, 2, 2, 2, 2, 2, 1, 2, 2, 1, 2, 2, 2, 2, 1, 2, 2, 1, 2, 2, 4 ),
 ( 0.7695219113824839363, 0.7713661461956111687, 0.7722882636021747293, 0.7725187929538156473, 0.7726340576296361062, 0.7726916899675463357, 0.7727493223054565652, 0.7732103810087384010, 0.7741324984153019617, 0.7745935571185837976, 0.7747088217944042565, 0.7747376379633593713, 0.7747664541323144860, 0.7748240864702247155, 0.7750546158218656334, 0.7759767332284291941, 0.7764377919317110299, 0.7766683212833518368, 0.7767259536212620663, 0.7767403617057396792, 0.7767475657479784301, 0.7767547697902171810, 0.7767835859591722958, 0.7768988506349927547, 0.7778209680415559824, 0.7787430854481192100, 0.7787574935325967118, 0.7787719016170743247, 0.7788007177860294394, 0.7788583501239395579, 0.7789736147997600169, 0.7792041441514008238, 0.7796652028546823265, 0.7805873202612454431, 0.7807025849370659021, 0.7807602172749760205, 0.7807890334439311353, 0.7808034415284087482, 0.7808178496128862500, 0.7810483789645270569, 0.7815094376678085597, 0.7824315550743716763, 0.7826620844260124832, 0.7827773491018328311, 0.7828061652707879459, 0.7828349814397430606, 0.7828926137776531791, 0.7833536724809347929, 0.7838147311842162956, 0.7839299958600367546, 0.7840452605358571025, 0.7842757898874979094, 0.7847368485907794122, 0.7848521132665998712, 0.7848809294355548749, 0.7849097456045099896, 0.7849673779424202191, 0.7851979072940610260, 0.7861200247006241426, 0.7865810834039056454, 0.7868116127555464523, 0.7868692450934566818, 0.7869268774313668002, 0.7870421421071872592, 0.7879642595137503758, 0.7888863769203133813, 0.7889151930892684961, 0.7889296011737461090, 0.7889440092582236108, 0.7890016415961338403, 0.7891169062719541882, 0.7893474356235949951, 0.7898084943268767200, 0.7907306117334399476, 0.7908458764092602955, 0.7909035087471705250, 0.7909323249161256397, 0.7909467330006031416, 0.7909539370428418925, 0.7909611410850807545, 0.7911916704367216724, 0.7916527291400033972, 0.7925748465465670689, 0.7928053758982079868, 0.7929206405740284458, 0.7929494567429835605, 0.7929638648274611734, 0.7929782729119386753, 0.7930359052498489048, 0.7934969639531307406, 0.7944190813596944123, 0.7948801400629762481, 0.7949954047387967071, 0.7950530370767069366, 0.7951106694146171661, 0.7953411987662580840, 0.7958022574695399198, 0.7959175221453603788, 0.7959751544832706083, 0.7960327868211808378, 0.7962633161728217557, 0.7967243748761035915, 0.7969549042277445094, 0.7970125365656547389, 0.7970413527346098537, 0.7970701689035649684, 0.7971854335793854274, 0.7981075509859490991, 0.7990296683925127708 ),
 .UNSPECIFIED. ) ;
#6963 = CARTESIAN_POINT ( 'NONE',  ( 7.714727599200456254, -62.47187499999984084, -18.62499999999935341 ) ) ;
#6964 = CARTESIAN_POINT ( 'NONE',  ( -9.084995278830836796, 67.53291598612975122, -9.998823687146330741 ) ) ;
#6965 = CARTESIAN_POINT ( 'NONE',  ( -18.62500000000064659, -52.06562499999986926, 7.714727599197333419 ) ) ;
#6966 = CARTESIAN_POINT ( 'NONE',  ( 12.91186397080207549, 54.28858565486373067, 3.944841525484266587 ) ) ;
#6967 = CARTESIAN_POINT ( 'NONE',  ( -10.31666293591003480, 64.59608009038818466, -8.707265613171941254 ) ) ;
#6968 = ORIENTED_EDGE ( 'NONE', *, *, #10040, .T. ) ;
#6969 = CARTESIAN_POINT ( 'NONE',  ( 11.00000000000001599, 0.000000000000000000, -15.58845726811988364 ) ) ;
#6970 = CARTESIAN_POINT ( 'NONE',  ( -13.46595428245841042, 34.89684888571769505, -0.9600937702945907537 ) ) ;
#6971 = ORIENTED_EDGE ( 'NONE', *, *, #6676, .F. ) ;
#6972 = CARTESIAN_POINT ( 'NONE',  ( 13.47848861578399138, 78.45635379196389181, -0.7637651279454616970 ) ) ;
#6973 = FACE_OUTER_BOUND ( 'NONE', #2307, .T. ) ;
#6974 = AXIS2_PLACEMENT_3D ( 'NONE', #737, #8711, #16813 ) ;
#6975 = DIRECTION ( 'NONE',  ( 0.000000000000000000, 0.000000000000000000, 1.000000000000000000 ) ) ;
#6976 = CARTESIAN_POINT ( 'NONE',  ( 11.00000000000001599, 0.000000000000000000, -15.58845726811988364 ) ) ;
#6977 = CARTESIAN_POINT ( 'NONE',  ( 4.754929249172622718, 73.00875652715450315, -12.63496230640105189 ) ) ;
#6978 = CARTESIAN_POINT ( 'NONE',  ( 21.14483242576213584, 7.170662809914417402, 2.970370385949366199 ) ) ;
#6979 = EDGE_CURVE ( 'NONE', #7754, #14613, #3048, .T. ) ;
#6980 = CARTESIAN_POINT ( 'NONE',  ( 4.171729424061791924, -18.97000000000000242, -12.83926296998457239 ) ) ;
#6981 = CARTESIAN_POINT ( 'NONE',  ( 4.171729424061789260, 74.83000000000001251, 12.83926296998457417 ) ) ;
#6982 = CARTESIAN_POINT ( 'NONE',  ( -11.24005743194561546, 52.64918859648530969, -7.477416982239327936 ) ) ;
#6983 = CARTESIAN_POINT ( 'NONE',  ( 9.520470885617717371, 43.72999999999999687, -6.917026985038131848 ) ) ;
#6984 = CARTESIAN_POINT ( 'NONE',  ( -8.343458848123582072, 67.37999999999998124, 11.48378591275254124 ) ) ;
#6985 = DIRECTION ( 'NONE',  ( 1.075706766891313654E-14, 0.000000000000000000, -1.000000000000000000 ) ) ;
#6986 = CARTESIAN_POINT ( 'NONE',  ( 11.61110246750533292, 69.17349466423988247, 6.887194277108547702 ) ) ;
#6987 = CARTESIAN_POINT ( 'NONE',  ( 12.00000000000002665, 2.413974596215582746, 3.899036354794885639 ) ) ;
#6988 = CARTESIAN_POINT ( 'NONE',  ( 12.00000000000000178, 5.296025403784440755, 1.734723475976807094E-15 ) ) ;
#6989 = CARTESIAN_POINT ( 'NONE',  ( 8.043339635997652337, -92.58124999999978400, -8.043339635996302306 ) ) ;
#6990 = CARTESIAN_POINT ( 'NONE',  ( -13.08483029837249845, 74.04834311179649831, 3.325739040386578971 ) ) ;
#6991 = CARTESIAN_POINT ( 'NONE',  ( -11.07543414285489902, 76.63905281824719395, -7.719769595326448020 ) ) ;
#6992 = DIRECTION ( 'NONE',  ( 0.000000000000000000, 1.000000000000000000, 0.000000000000000000 ) ) ;
#6993 = CARTESIAN_POINT ( 'NONE',  ( -9.708203932499369415, 0.4960254037844292752, -7.053423027509682086 ) ) ;
#6994 = CYLINDRICAL_SURFACE ( 'NONE', #80, 12.00000000000000178 ) ;
#6995 = CARTESIAN_POINT ( 'NONE',  ( 15.00000000000000000, 0.000000000000000000, 1.256933281983527907E-12 ) ) ;
#6996 = CARTESIAN_POINT ( 'NONE',  ( -11.76794919243112325, -2.220000000000004192, -3.823638476888998827 ) ) ;
#6997 = CARTESIAN_POINT ( 'NONE',  ( -7.272992578804310604, 51.37999999999998835, 10.01041549318726886 ) ) ;
#6998 = CARTESIAN_POINT ( 'NONE',  ( -10.92172942406179104, 2.230000000000009752, 7.935100905948385908 ) ) ;
#6999 = PLANE ( 'NONE',  #5181 ) ;
#7000 = CARTESIAN_POINT ( 'NONE',  ( 10.94004585081460768, 75.13044969108922544, 7.925841433480270481 ) ) ;
#7001 = EDGE_CURVE ( 'NONE', #4482, #8166, #3906, .T. ) ;
#7002 = CARTESIAN_POINT ( 'NONE',  ( 8.627630420782578469, 5.967892910702088472E-16, -8.354871048539219913 ) ) ;
#7003 = CARTESIAN_POINT ( 'NONE',  ( -7.576616670048093940E-16, 33.67999999999999972, 12.37355403259654985 ) ) ;
#7004 = CARTESIAN_POINT ( 'NONE',  ( -4.368811843459432964, 41.52287850255721935, 12.77356621052920893 ) ) ;
#7005 = CARTESIAN_POINT ( 'NONE',  ( 5.349201313263153068, 51.98641939972569759, -12.39963371175743490 ) ) ;
#7006 = CARTESIAN_POINT ( 'NONE',  ( -7.122634015147881748, 38.41518589931285987, 11.46826829916993873 ) ) ;
#7007 = CARTESIAN_POINT ( 'NONE',  ( -8.343458848123578520, 54.48000000000001108, -11.48378591275254124 ) ) ;
#7008 = CARTESIAN_POINT ( 'NONE',  ( -4.171729424061791036, 5.530000000000007354, 12.83926296998457239 ) ) ;
#7009 = CARTESIAN_POINT ( 'NONE',  ( -7.416407864998755706, 1.513974596215569957, 10.20780970022450163 ) ) ;
#7010 = CARTESIAN_POINT ( 'NONE',  ( -6.622037744496604539, 49.42396662578299527, -11.76708925107785753 ) ) ;
#7011 = CARTESIAN_POINT ( 'NONE',  ( 11.53816879259289685, 63.16854332020811569, 7.008656503616835565 ) ) ;
#7012 = CARTESIAN_POINT ( 'NONE',  ( 10.32716819451351498, 42.09648712927666736, 8.701702194760818188 ) ) ;
#7013 = CARTESIAN_POINT ( 'NONE',  ( 5.937526285386327984, 48.96352261484946666, -12.12418171604482353 ) ) ;
#7014 = EDGE_LOOP ( 'NONE', ( #11832, #651, #906, #2870 ) ) ;
#7015 = CARTESIAN_POINT ( 'NONE',  ( -9.520470885617715595, 74.62999999999999545, -6.917026985038136289 ) ) ;
#7016 = DIRECTION ( 'NONE',  ( -0.000000000000000000, -1.000000000000000000, -0.000000000000000000 ) ) ;
#7017 = DIRECTION ( 'NONE',  ( -0.000000000000000000, 1.000000000000000000, -0.000000000000000000 ) ) ;
#7018 = CARTESIAN_POINT ( 'NONE',  ( -13.49999999999999822, 7.779999999999992255, -4.386415899144240349 ) ) ;
#7019 = ORIENTED_EDGE ( 'NONE', *, *, #2974, .T. ) ;
#7020 = CARTESIAN_POINT ( 'NONE',  ( -11.53224498248871122, 43.66710377932096776, -7.048982063341345139 ) ) ;
#7021 = CARTESIAN_POINT ( 'NONE',  ( -7.500000000000000000, 107.4971863040494213, 6.484415072061723961 ) ) ;
#7022 = CARTESIAN_POINT ( 'NONE',  ( 6.365913562993081420, 60.94642428639450316, -11.90484108844855804 ) ) ;
#7023 = CARTESIAN_POINT ( 'NONE',  ( 2.621994543952811015E-15, 11.18000000000000149, -14.19474002721660355 ) ) ;
#7024 = EDGE_CURVE ( 'NONE', #14888, #1687, #9230, .T. ) ;
#7025 = CARTESIAN_POINT ( 'NONE',  ( 18.62500000000000000, 0.000000000000000000, 1.560692158462880521E-12 ) ) ;
#7026 = CARTESIAN_POINT ( 'NONE',  ( 13.50062667129575722, 66.42363412073690654, 0.1755086108962339297 ) ) ;
#7027 = CARTESIAN_POINT ( 'NONE',  ( 1.467847692288238193, 56.73277838508402482, 13.41996759063894373 ) ) ;
#7028 = CARTESIAN_POINT ( 'NONE',  ( 9.520470885617715595, 64.12999999999999545, 6.917026985038134512 ) ) ;
#7029 = CARTESIAN_POINT ( 'NONE',  ( -3.636496289402153081, 68.32999999999999829, -11.19198476289190936 ) ) ;
#7030 = CARTESIAN_POINT ( 'NONE',  ( -13.49150454620358275, 46.94646972587323575, 0.4788601354586907166 ) ) ;
#7031 = FACE_OUTER_BOUND ( 'NONE', #11935, .T. ) ;
#7032 = CARTESIAN_POINT ( 'NONE',  ( 2.138189944381248875, 73.75688142232027644, 13.49999999999999645 ) ) ;
#7033 = CARTESIAN_POINT ( 'NONE',  ( 9.477935110687690567, 30.80768188101512806, -9.621815863905913702 ) ) ;
#7034 = VECTOR ( 'NONE', #10653, 1000.000000000000000 ) ;
#7035 = CARTESIAN_POINT ( 'NONE',  ( -3.315231683446368205, 56.56075311393848182, 13.08712957443356117 ) ) ;
#7036 = CARTESIAN_POINT ( 'NONE',  ( -8.043339635997654113, -60.35624999999985363, 8.043339635996302306 ) ) ;
#7037 = CARTESIAN_POINT ( 'NONE',  ( 10.92172942406179104, 6.730000000000013749, -7.935100905948385908 ) ) ;
#7038 = CARTESIAN_POINT ( 'NONE',  ( 11.44289832574866139, 33.69789852399187424, -7.163812845423511710 ) ) ;
#7039 = CARTESIAN_POINT ( 'NONE',  ( -4.491212130746389697, 10.00000000000000000, 11.83243654515264076 ) ) ;
#7040 = DIRECTION ( 'NONE',  ( 0.000000000000000000, 1.000000000000000000, 0.000000000000000000 ) ) ;
#7041 = CARTESIAN_POINT ( 'NONE',  ( 9.520470885617715595, 23.13000000000001322, 6.917026985038135400 ) ) ;
#7042 = EDGE_LOOP ( 'NONE', ( #8194, #4742, #9280, #5977 ) ) ;
#7043 = CARTESIAN_POINT ( 'NONE',  ( -4.489940415681219044, 62.51839048220814021, 12.73204617180344300 ) ) ;
#7044 = ORIENTED_EDGE ( 'NONE', *, *, #4192, .F. ) ;
#7045 = CARTESIAN_POINT ( 'NONE',  ( -3.636496289402156190, -16.46999999999999886, 11.19198476289190758 ) ) ;
#7046 = CARTESIAN_POINT ( 'NONE',  ( 7.714727599200456254, -43.67187499999991473, -18.62499999999935341 ) ) ;
#7047 = CARTESIAN_POINT ( 'NONE',  ( -13.47256314982935166, 43.95974442004008154, 0.8609111014920134419 ) ) ;
#7048 = CARTESIAN_POINT ( 'NONE',  ( 0.000000000000000000, -8.000000000000000000, 0.000000000000000000 ) ) ;
#7049 = CARTESIAN_POINT ( 'NONE',  ( 8.343458848123578520, 32.97999999999999687, 11.48378591275254124 ) ) ;
#7050 = CARTESIAN_POINT ( 'NONE',  ( 1.708800344670653191E-06, 35.68004753840243382, 13.49999999999978328 ) ) ;
#7051 = CARTESIAN_POINT ( 'NONE',  ( -5.995605309098753999, 67.39875943548146608, -12.09707223761978412 ) ) ;
#7052 = CARTESIAN_POINT ( 'NONE',  ( -18.62499999999935341, -83.28437499999976978, -7.714727599200458030 ) ) ;
#7053 = CARTESIAN_POINT ( 'NONE',  ( 11.53575417012443616, 54.69162266907183323, -7.012590288925422577 ) ) ;
#7054 = ADVANCED_FACE ( 'NONE', ( #7069 ), #4584, .F. ) ;
#7055 = CARTESIAN_POINT ( 'NONE',  ( -9.572234266482416487, 64.55715410289911915, -9.527515327432464431 ) ) ;
#7056 = EDGE_LOOP ( 'NONE', ( #1357, #13789, #11098, #5602 ) ) ;
#7057 = CARTESIAN_POINT ( 'NONE',  ( -13.38605536481362890, 34.99161834286027783, 1.764857785377393684 ) ) ;
#7058 = EDGE_LOOP ( 'NONE', ( #7779, #14417, #15222, #10173 ) ) ;
#7059 = CARTESIAN_POINT ( 'NONE',  ( 11.85483473061306015, 78.19086039256470144, 6.458558312265882506 ) ) ;
#7060 = CARTESIAN_POINT ( 'NONE',  ( 13.50000000000000355, 47.57999999999999119, -4.386415899144233244 ) ) ;
#7061 = CARTESIAN_POINT ( 'NONE',  ( 7.500000000000003553, -27.44685421792581792, 4.091673783487185467 ) ) ;
#7062 = CARTESIAN_POINT ( 'NONE',  ( 5.236401750311364900, 72.99073825183825193, -12.44474146415180904 ) ) ;
#7063 = CARTESIAN_POINT ( 'NONE',  ( 1.086230788847387219, 79.14096883825459372, -13.45868988004304612 ) ) ;
#7064 = CARTESIAN_POINT ( 'NONE',  ( 10.92172942406179104, -16.26999999999999957, -7.935100905948385908 ) ) ;
#7065 = CARTESIAN_POINT ( 'NONE',  ( 13.50000000000000355, 60.57999999999998408, -4.386415899144233244 ) ) ;
#7066 = CARTESIAN_POINT ( 'NONE',  ( -13.00272673885899266, 53.06012234098268721, 3.637067801120180022 ) ) ;
#7067 = CARTESIAN_POINT ( 'NONE',  ( 11.76794919243112325, 40.27999999999998693, 3.823638476888996607 ) ) ;
#7068 = CARTESIAN_POINT ( 'NONE',  ( -8.343458848123582072, 58.38000000000000256, 11.48378591275254124 ) ) ;
#7069 = FACE_OUTER_BOUND ( 'NONE', #8525, .T. ) ;
#7070 = CARTESIAN_POINT ( 'NONE',  ( 12.70536037991022305, 69.26510775276948095, 4.563833866671145323 ) ) ;
#7071 = CARTESIAN_POINT ( 'NONE',  ( -2.012210829378426435, 37.25231257445182109, -13.35686934311003959 ) ) ;
#7072 = CARTESIAN_POINT ( 'NONE',  ( 2.902084407815607718E-14, 5.180000000000006821, -13.50000000000000000 ) ) ;
#7073 = CARTESIAN_POINT ( 'NONE',  ( 13.16986379959833897, -71.76874999999985505, 13.16986379960055409 ) ) ;
#7074 = CARTESIAN_POINT ( 'NONE',  ( -10.25778635652197224, 74.26711310232562369, 8.777052303075189243 ) ) ;
#7075 = CARTESIAN_POINT ( 'NONE',  ( -4.990650801110085411, 76.36006663702048058, -12.54403061954694110 ) ) ;
#7076 = CARTESIAN_POINT ( 'NONE',  ( -0.1775006636059834053, 8.062177826491096155, -17.99999999999999289 ) ) ;
#7077 = CARTESIAN_POINT ( 'NONE',  ( 0.000000000000000000, 80.93000000000000682, 0.000000000000000000 ) ) ;
#7078 = CARTESIAN_POINT ( 'NONE',  ( -11.42802927808057767, 80.93000000000002103, 3.799729825752809820 ) ) ;
#7079 = DIRECTION ( 'NONE',  ( -1.000000000000000000, 0.000000000000000000, -8.379555213223520053E-14 ) ) ;
#7080 = CARTESIAN_POINT ( 'NONE',  ( 3.636496289402154414, -7.169999999999995488, 11.19198476289190758 ) ) ;
#7081 = CARTESIAN_POINT ( 'NONE',  ( -7.272992578804310604, 33.38000000000000256, 10.01041549318726886 ) ) ;
#7082 = CARTESIAN_POINT ( 'NONE',  ( 8.343458848123578520, -15.02000000000000846, 11.48378591275254124 ) ) ;
#7083 = CARTESIAN_POINT ( 'NONE',  ( -8.740054970619736352, 32.34338933063859400, 10.29130291274103470 ) ) ;
#7084 = CARTESIAN_POINT ( 'NONE',  ( 12.75897847405612318, 75.26823319679101587, 4.501030925202505806 ) ) ;
#7085 = CARTESIAN_POINT ( 'NONE',  ( 4.295984800146390725, -1.623771540349147248E-16, -12.82069415802188672 ) ) ;
#7086 = CARTESIAN_POINT ( 'NONE',  ( -11.76794919243112325, 32.77999999999999403, -3.823638476888998827 ) ) ;
#7087 = AXIS2_PLACEMENT_3D ( 'NONE', #3462, #11515, #12749 ) ;
#7088 = CARTESIAN_POINT ( 'NONE',  ( 0.5526492435590804053, 52.16013233706370045, -13.49040056943439581 ) ) ;
#7089 = CARTESIAN_POINT ( 'NONE',  ( 0.000000000000000000, 5.918584287042170544, 0.000000000000000000 ) ) ;
#7090 = CARTESIAN_POINT ( 'NONE',  ( 0.09524022798341912066, 37.17657551321138953, -13.49966522572602301 ) ) ;
#7091 = CARTESIAN_POINT ( 'NONE',  ( -16.82677684650015237, 7.170662809914417402, -13.14483242576234723 ) ) ;
#7092 = EDGE_CURVE ( 'NONE', #13300, #5695, #12220, .T. ) ;
#7093 = DIRECTION ( 'NONE',  ( 0.000000000000000000, 0.000000000000000000, 1.000000000000000000 ) ) ;
#7094 = CARTESIAN_POINT ( 'NONE',  ( 12.18353207652669923, 63.21590633337540055, 5.835071146089095606 ) ) ;
#7095 = CARTESIAN_POINT ( 'NONE',  ( 13.21374623997747122, 42.52811597142575550, -2.775631991069858806 ) ) ;
#7096 = CARTESIAN_POINT ( 'NONE',  ( 5.970456528392105611, 48.96224137250303698, -12.10801974513590906 ) ) ;
#7097 = CARTESIAN_POINT ( 'NONE',  ( -7.409984580736203970E-16, 22.68000000000000327, 12.37355403259654985 ) ) ;
#7098 = ORIENTED_EDGE ( 'NONE', *, *, #5375, .T. ) ;
#7099 = CARTESIAN_POINT ( 'NONE',  ( -9.520470885617715595, 71.62999999999999545, -6.917026985038136289 ) ) ;
#7100 = DIRECTION ( 'NONE',  ( 0.000000000000000000, 0.000000000000000000, 1.000000000000000000 ) ) ;
#7101 = CARTESIAN_POINT ( 'NONE',  ( 11.37499999999960210, -65.55937499999983231, 4.711679271994917428 ) ) ;
#7102 = CARTESIAN_POINT ( 'NONE',  ( -8.343458848123576743, 4.480000000000009308, -11.48378591275254301 ) ) ;
#7103 = EDGE_LOOP ( 'NONE', ( #1682, #10561, #16383, #16909 ) ) ;
#7104 = CARTESIAN_POINT ( 'NONE',  ( -6.177155207478421062, 43.40604133974412093, -12.00656696816257885 ) ) ;
#7105 = CARTESIAN_POINT ( 'NONE',  ( -7.499999999999997335, 105.3828822090421085, 8.693347190813732084 ) ) ;
#7106 = CARTESIAN_POINT ( 'NONE',  ( 13.10225137871006673, 60.54575384758864232, -3.255519868551609353 ) ) ;
#7107 = CARTESIAN_POINT ( 'NONE',  ( 4.171729424061791924, 5.030000000000006466, -12.83926296998457239 ) ) ;
#7108 = CARTESIAN_POINT ( 'NONE',  ( -7.416407864998736166, 6.346025403784442354, -10.20780970022448031 ) ) ;
#7109 = CARTESIAN_POINT ( 'NONE',  ( 11.78404408794452074, 66.18568652898561311, 6.586852905507519118 ) ) ;
#7110 = CARTESIAN_POINT ( 'NONE',  ( 3.262996936836821682, 56.79731715246284551, 13.09972757844540858 ) ) ;
#7111 = CARTESIAN_POINT ( 'NONE',  ( -11.76794919243112325, 62.92999999999999972, -2.882316262207890869E-15 ) ) ;
#7112 = CARTESIAN_POINT ( 'NONE',  ( -11.76794919243112325, 66.07999999999999829, 3.823638476888994386 ) ) ;
#7113 = CARTESIAN_POINT ( 'NONE',  ( -12.65132248824962602, 46.75933051274522256, -4.715090284878137972 ) ) ;
#7114 = CARTESIAN_POINT ( 'NONE',  ( 12.41168389898173707, 45.62405102665109524, -5.326589421794383661 ) ) ;
#7115 = CARTESIAN_POINT ( 'NONE',  ( 10.92172942406178926, 74.12999999999999545, 7.935100905948387684 ) ) ;
#7116 = CARTESIAN_POINT ( 'NONE',  ( 1.468262939039568948, 31.12731509695948873, -13.42493789908898094 ) ) ;
#7117 = CARTESIAN_POINT ( 'NONE',  ( -2.973838119809171232, 56.57298728218007966, 13.17046594805706050 ) ) ;
#7118 = CARTESIAN_POINT ( 'NONE',  ( 9.538709233711902776E-13, -87.41249999999979536, -11.37500000000000000 ) ) ;
#7119 = CARTESIAN_POINT ( 'NONE',  ( 2.138189944381200469, 7.103118577679737200, -13.50000000000001421 ) ) ;
#7120 = CARTESIAN_POINT ( 'NONE',  ( 8.740325781130335869, 33.01677564961078559, 10.29107445509964336 ) ) ;
#7121 = DIRECTION ( 'NONE',  ( 0.000000000000000000, 0.000000000000000000, 1.000000000000000000 ) ) ;
#7122 = CARTESIAN_POINT ( 'NONE',  ( 4.295754402788634962, 40.02552785855749562, -12.79831863505647860 ) ) ;
#7123 = CARTESIAN_POINT ( 'NONE',  ( -11.76794919243112325, 21.93000000000000682, -2.602085213965210642E-15 ) ) ;
#7124 = ORIENTED_EDGE ( 'NONE', *, *, #5724, .T. ) ;
#7125 = CARTESIAN_POINT ( 'NONE',  ( -9.353866460873140554, 62.31375578855443109, 9.736707939222794650 ) ) ;
#7126 = VERTEX_POINT ( 'NONE', #10244 ) ;
#7127 = CARTESIAN_POINT ( 'NONE',  ( -1.564113515457998370E-12, -19.73749999999997229, 18.62500000000000000 ) ) ;
#7128 = CARTESIAN_POINT ( 'NONE',  ( -13.24414797687638057, 44.02231978228942921, 2.615972014630898457 ) ) ;
#7129 = CIRCLE ( 'NONE', #13045, 1.999999999999998224 ) ;
#7130 = CARTESIAN_POINT ( 'NONE',  ( 10.92172942406179104, 65.72999999999998977, -7.935100905948385908 ) ) ;
#7131 = CARTESIAN_POINT ( 'NONE',  ( -9.520470885617715595, 83.62999999999999545, -6.917026985038136289 ) ) ;
#7132 = CARTESIAN_POINT ( 'NONE',  ( -4.171729424061787483, 48.32999999999999829, -12.83926296998457417 ) ) ;
#7133 = CARTESIAN_POINT ( 'NONE',  ( -6.200018879092032975, 46.40684524066041661, -11.99220497138590602 ) ) ;
#7134 = CARTESIAN_POINT ( 'NONE',  ( -11.15157066607664049, 67.64369004200317192, -7.609460659245025127 ) ) ;
#7135 = CARTESIAN_POINT ( 'NONE',  ( 11.37500000000000178, 7.250000000000001776, 9.531744055041752924E-13 ) ) ;
#7136 = AXIS2_PLACEMENT_3D ( 'NONE', #15022, #1600, #9758 ) ;
#7137 = ADVANCED_FACE ( 'NONE', ( #11392 ), #5621, .T. ) ;
#7138 = CARTESIAN_POINT ( 'NONE',  ( 11.05849770819798117, 54.13800262379849215, 7.750384364272157711 ) ) ;
#7139 = CARTESIAN_POINT ( 'NONE',  ( -10.33389146060662078, 64.59699217978335639, -8.686821934247454635 ) ) ;
#7140 = ORIENTED_EDGE ( 'NONE', *, *, #4192, .T. ) ;
#7141 = CARTESIAN_POINT ( 'NONE',  ( -8.388358401731302649, 34.50044823484911660, -10.57791826008529767 ) ) ;
#7142 = CARTESIAN_POINT ( 'NONE',  ( 11.37499999999960210, -65.55937499999984652, 4.711679271994918317 ) ) ;
#7143 = CARTESIAN_POINT ( 'NONE',  ( 11.87658369898086086, 78.19247217947236095, 6.418497554539179362 ) ) ;
#7144 = DIRECTION ( 'NONE',  ( -1.000000000000000000, -1.734723475976807094E-16, -0.000000000000000000 ) ) ;
#7145 = CARTESIAN_POINT ( 'NONE',  ( 7.500000000000000888, -27.79580463407382496, 1.043242051446493734 ) ) ;
#7146 = CARTESIAN_POINT ( 'NONE',  ( 12.77798252166430792, 72.27295531305313148, 4.357763951314068684 ) ) ;
#7147 = CARTESIAN_POINT ( 'NONE',  ( 4.953551091470167478, 79.00132416387516798, -12.55835749735045859 ) ) ;
#7148 = CARTESIAN_POINT ( 'NONE',  ( -11.76794919243112325, 33.78000000000000824, -3.823638476888998827 ) ) ;
#7149 = CARTESIAN_POINT ( 'NONE',  ( -10.92172942406178926, 58.63000000000000256, -7.935100905948389460 ) ) ;
#7150 = CARTESIAN_POINT ( 'NONE',  ( -13.49426538080809834, 52.94671897916216352, 0.4876541610707976759 ) ) ;
#7151 = VECTOR ( 'NONE', #5944, 1000.000000000000000 ) ;
#7152 = CARTESIAN_POINT ( 'NONE',  ( 9.520470885617715595, 37.12999999999999545, 6.917026985038134512 ) ) ;
#7153 = CARTESIAN_POINT ( 'NONE',  ( 13.49999999999999822, 56.27999999999999403, 4.386415899144237684 ) ) ;
#7154 = CARTESIAN_POINT ( 'NONE',  ( 2.138189944381236884, 78.10311857767972299, -13.50000000000000000 ) ) ;
#7155 = CARTESIAN_POINT ( 'NONE',  ( 9.520470885617717371, -6.269999999999997797, -6.917026985038131848 ) ) ;
#7156 = CARTESIAN_POINT ( 'NONE',  ( 3.700846756827888218, 68.81299210504440111, 12.98334767858451677 ) ) ;
#7157 = CARTESIAN_POINT ( 'NONE',  ( -0.2970657467180017886, 37.19068138831143955, -13.50000000000001066 ) ) ;
#7158 = CARTESIAN_POINT ( 'NONE',  ( 0.000000000000000000, 9.000000000000000000, 0.000000000000000000 ) ) ;
#7159 = CARTESIAN_POINT ( 'NONE',  ( 7.714727599197340524, -54.07812499999989342, 18.62500000000063949 ) ) ;
#7160 = CARTESIAN_POINT ( 'NONE',  ( -12.51477381949817413, 73.74582926830240126, -5.065646498870927772 ) ) ;
#7161 = CARTESIAN_POINT ( 'NONE',  ( -2.278090379941454025, 76.26191102292980872, -13.30664668557865760 ) ) ;
#7162 = FACE_OUTER_BOUND ( 'NONE', #15, .T. ) ;
#7163 = CARTESIAN_POINT ( 'NONE',  ( -3.708203932499370303, 1.396025403784441066, 11.41267819554184371 ) ) ;
#7164 = CARTESIAN_POINT ( 'NONE',  ( 0.000000000000000000, -28.00000000000000000, 0.000000000000000000 ) ) ;
#7165 = CARTESIAN_POINT ( 'NONE',  ( -7.272992578804307939, -5.520000000000001350, -10.01041549318726886 ) ) ;
#7166 = CARTESIAN_POINT ( 'NONE',  ( 3.636496289402157078, 35.03000000000000114, -11.19198476289190936 ) ) ;
#7167 = CARTESIAN_POINT ( 'NONE',  ( -13.49999999999999822, -13.21999999999999709, -4.386415899144240349 ) ) ;
#7168 = CARTESIAN_POINT ( 'NONE',  ( -9.429961120686421339, 32.30986108813164037, 9.660530610400291707 ) ) ;
#7169 = CARTESIAN_POINT ( 'NONE',  ( 13.32338872245472849, 75.35360622757792726, 2.176581829586916594 ) ) ;
#7170 = CARTESIAN_POINT ( 'NONE',  ( 5.292333123709091147, 1.381986750645590742E-15, -11.92816106025346556 ) ) ;
#7171 = CARTESIAN_POINT ( 'NONE',  ( -3.636496289402153081, 32.32999999999999829, -11.19198476289190936 ) ) ;
#7172 = CARTESIAN_POINT ( 'NONE',  ( 10.04873594665206937, 51.77822116537775088, -9.015151377439948988 ) ) ;
#7173 = CARTESIAN_POINT ( 'NONE',  ( -4.644322785898420847, 38.51283592794423072, 12.67769253242001959 ) ) ;
#7174 = CARTESIAN_POINT ( 'NONE',  ( 6.594030187424503531, 36.93740925139908171, -11.79378183334034880 ) ) ;
#7175 = CARTESIAN_POINT ( 'NONE',  ( 0.000000000000000000, 3.999999999999961808, 0.000000000000000000 ) ) ;
#7176 = FACE_OUTER_BOUND ( 'NONE', #7555, .T. ) ;
#7177 = CARTESIAN_POINT ( 'NONE',  ( 7.072526022525592815, 62.94270560853125573, 11.49911144502164895 ) ) ;
#7178 = CARTESIAN_POINT ( 'NONE',  ( 12.46071941648464332, 42.24086282136816095, 5.195455325495793808 ) ) ;
#7179 = CARTESIAN_POINT ( 'NONE',  ( 13.30280394725709314, 48.51140726369936829, -2.319129228756254157 ) ) ;
#7180 = CARTESIAN_POINT ( 'NONE',  ( 9.520470885617715595, 20.13000000000000966, 6.917026985038135400 ) ) ;
#7181 = ORIENTED_EDGE ( 'NONE', *, *, #10188, .F. ) ;
#7182 = CARTESIAN_POINT ( 'NONE',  ( 3.636496289402154414, 69.82999999999999829, 11.19198476289190936 ) ) ;
#7183 = CARTESIAN_POINT ( 'NONE',  ( -1.564113515457998370E-12, -88.48749999999975557, 18.62500000000000000 ) ) ;
#7184 = CARTESIAN_POINT ( 'NONE',  ( -4.711679271994915652, -28.09687499999992966, 11.37499999999960210 ) ) ;
#7185 = ORIENTED_EDGE ( 'NONE', *, *, #5899, .T. ) ;
#7186 = CARTESIAN_POINT ( 'NONE',  ( -10.09708985121333136, 43.58387330091565559, -8.971927331284039298 ) ) ;
#7187 = LINE ( 'NONE', #12576, #9100 ) ;
#7188 = CARTESIAN_POINT ( 'NONE',  ( -13.49999999999999822, 2.779999999999990923, -4.386415899144240349 ) ) ;
#7189 = CARTESIAN_POINT ( 'NONE',  ( -18.62500000000064659, -9.365624999999976552, 7.714727599197333419 ) ) ;
#7190 = CARTESIAN_POINT ( 'NONE',  ( 11.79401460576306526, 66.18640916527446905, 6.568962329648897480 ) ) ;
#7191 = CARTESIAN_POINT ( 'NONE',  ( 10.77767612607841485, 57.12170114078097782, 8.130105570404699833 ) ) ;
#7192 = ADVANCED_FACE ( 'NONE', ( #11563 ), #1910, .F. ) ;
#7193 = CARTESIAN_POINT ( 'NONE',  ( 3.636496289402154414, 63.82999999999999829, 11.19198476289190936 ) ) ;
#7194 = CARTESIAN_POINT ( 'NONE',  ( 13.49999999999999822, 32.27999999999999403, 4.386415899144237684 ) ) ;
#7195 = CARTESIAN_POINT ( 'NONE',  ( -3.636496289402155746, 66.53000000000000114, 11.19198476289190936 ) ) ;
#7196 = CARTESIAN_POINT ( 'NONE',  ( -11.34494330406672624, 46.65582902796952425, -7.317300534094159481 ) ) ;
#7197 = CARTESIAN_POINT ( 'NONE',  ( 5.569239368393173351, 45.97791013593247555, -12.29771055457881879 ) ) ;
#7198 = CARTESIAN_POINT ( 'NONE',  ( -4.023268246324633536E-14, 60.18000000000000682, -13.50000000000000000 ) ) ;
#7199 = PRESENTATION_STYLE_ASSIGNMENT (( #1702 ) ) ;
#7200 = CARTESIAN_POINT ( 'NONE',  ( 0.06185192672290352328, 31.17777603289167843, -13.49999999999999467 ) ) ;
#7201 = CARTESIAN_POINT ( 'NONE',  ( 17.32050807568878170, 0.000000000000000000, -7.999999999999961808 ) ) ;
#7202 = DIRECTION ( 'NONE',  ( -0.8660254037844434816, 0.000000000000000000, 0.4999999999999918399 ) ) ;
#7203 = CARTESIAN_POINT ( 'NONE',  ( 10.54218125873905443, 33.10822676551072163, 8.435822891053812000 ) ) ;
#7204 = CARTESIAN_POINT ( 'NONE',  ( -3.600152184539524125, 10.00000000000000000, 12.19664001577687173 ) ) ;
#7205 = CARTESIAN_POINT ( 'NONE',  ( 5.219660855938430544, 39.99127885146727834, -12.45468320406492069 ) ) ;
#7206 = ORIENTED_EDGE ( 'NONE', *, *, #5396, .T. ) ;
#7207 = CARTESIAN_POINT ( 'NONE',  ( -13.46448297031965247, 61.96386121747416098, 0.9786549340198757996 ) ) ;
#7208 = ORIENTED_EDGE ( 'NONE', *, *, #12672, .F. ) ;
#7209 = CARTESIAN_POINT ( 'NONE',  ( -13.49062013346076938, 40.94740657223831448, 0.5061247442112529749 ) ) ;
#7210 = CARTESIAN_POINT ( 'NONE',  ( 1.561832610794586740E-12, -78.01249999999983231, -18.62500000000000000 ) ) ;
#7211 = CARTESIAN_POINT ( 'NONE',  ( -12.43644091682779163, 44.12163909514725191, 5.256796654357501986 ) ) ;
#7212 = CARTESIAN_POINT ( 'NONE',  ( 4.171729424061791924, 66.03000000000000114, -12.83926296998457239 ) ) ;
#7213 = CARTESIAN_POINT ( 'NONE',  ( 13.49999999999999822, 33.27999999999999403, 4.386415899144237684 ) ) ;
#7214 = CARTESIAN_POINT ( 'NONE',  ( 2.607531440858944223E-15, 42.17999999999999261, -14.19474002721660355 ) ) ;
#7215 = EDGE_CURVE ( 'NONE', #568, #668, #14109, .T. ) ;
#7216 = CARTESIAN_POINT ( 'NONE',  ( -0.3512640400060916823, 8.055266896996092996, 18.02316420754749871 ) ) ;
#7217 = CARTESIAN_POINT ( 'NONE',  ( -8.495721255044264453, 67.50532034020808680, -10.49469503808201765 ) ) ;
#7218 = CARTESIAN_POINT ( 'NONE',  ( 4.711679271994911211, 4.128125000000008704, -11.37499999999960743 ) ) ;
#7219 = CARTESIAN_POINT ( 'NONE',  ( 8.925127373670504127, 54.02551875695034056, 10.13307151360432634 ) ) ;
#7220 = ORIENTED_EDGE ( 'NONE', *, *, #696, .F. ) ;
#7221 = CARTESIAN_POINT ( 'NONE',  ( -7.708711337361060956, 64.46994343615379819, -11.08696526454483333 ) ) ;
#7222 = VERTEX_POINT ( 'NONE', #7587 ) ;
#7223 = CYLINDRICAL_SURFACE ( 'NONE', #13417, 14.50000000000000000 ) ;
#7224 = CARTESIAN_POINT ( 'NONE',  ( -10.19850433080654639, 34.58972380950302750, -8.845366638170691687 ) ) ;
#7225 = CARTESIAN_POINT ( 'NONE',  ( 8.043339635996300530, -47.86874999999988489, 8.043339635997654113 ) ) ;
#7226 = CARTESIAN_POINT ( 'NONE',  ( 10.50252084001531117, 78.10619439663850017, 8.482238275819085516 ) ) ;
#7227 = CARTESIAN_POINT ( 'NONE',  ( -10.68887637698740534, 7.854719008739928121, -15.43480272504890571 ) ) ;
#7228 = CARTESIAN_POINT ( 'NONE',  ( 7.500000000000002665, -27.18121722713998523, -5.064597142177446720 ) ) ;
#7229 = CARTESIAN_POINT ( 'NONE',  ( 13.37722696026129832, 72.36650144554805308, 1.816547976767812322 ) ) ;
#7230 = CARTESIAN_POINT ( 'NONE',  ( 7.272992578804308828, 25.98000000000001108, 10.01041549318726709 ) ) ;
#7231 = CIRCLE ( 'NONE', #12017, 26.00000000000000355 ) ;
#7232 = CARTESIAN_POINT ( 'NONE',  ( 4.171729424061789260, 59.82999999999999119, 12.83926296998457417 ) ) ;
#7233 = CARTESIAN_POINT ( 'NONE',  ( -8.842990959453766564, 52.52165125223628195, -10.20056964289610058 ) ) ;
#7234 = EDGE_CURVE ( 'NONE', #13257, #17257, #13771, .T. ) ;
#7235 = CARTESIAN_POINT ( 'NONE',  ( 11.76794919243112325, 37.42999999999999972, 1.441158131103945434E-15 ) ) ;
#7236 = CARTESIAN_POINT ( 'NONE',  ( 8.343458848123583849, 59.87999999999998835, -11.48378591275253768 ) ) ;
#7237 = CARTESIAN_POINT ( 'NONE',  ( -15.78643792884158437, 8.055054264001460851, -8.704847339800664940 ) ) ;
#7238 = CARTESIAN_POINT ( 'NONE',  ( 9.520470885617715595, -3.869999999999998330, 6.917026985038135400 ) ) ;
#7239 = CARTESIAN_POINT ( 'NONE',  ( 11.75284362809797223, 69.18342969977395285, 6.642835211192756439 ) ) ;
#7240 = CARTESIAN_POINT ( 'NONE',  ( 0.000000000000000000, 30.93000000000001393, -13.50000000000000000 ) ) ;
#7241 = CARTESIAN_POINT ( 'NONE',  ( 1.395181907640911101, 35.73016548663857606, 13.42772203881113846 ) ) ;
#7242 = CARTESIAN_POINT ( 'NONE',  ( -13.16986379960055409, -84.25624999999983800, 13.16986379959834252 ) ) ;
#7243 = CARTESIAN_POINT ( 'NONE',  ( -13.48320498675965595, 73.90678838288567931, -0.6742141303992607027 ) ) ;
#7244 = VECTOR ( 'NONE', #6654, 1000.000000000000000 ) ;
#7245 = CARTESIAN_POINT ( 'NONE',  ( -4.659656022607111758, 76.34776334268970288, -12.67034846265207726 ) ) ;
#7246 = CYLINDRICAL_SURFACE ( 'NONE', #7899, 13.50000000000000000 ) ;
#7247 = LINE ( 'NONE', #13848, #12867 ) ;
#7248 = CARTESIAN_POINT ( 'NONE',  ( 9.739336723526609063, 8.018126783878129160, -15.33316801648999217 ) ) ;
#7249 = CARTESIAN_POINT ( 'NONE',  ( 13.50000000000000355, 28.58000000000000540, -4.386415899144233244 ) ) ;
#7250 = CARTESIAN_POINT ( 'NONE',  ( -3.636496289402156190, -4.469999999999994422, 11.19198476289190758 ) ) ;
#7251 = CARTESIAN_POINT ( 'NONE',  ( -11.76794919243112325, 42.07999999999999829, 3.823638476888994830 ) ) ;
#7252 = CARTESIAN_POINT ( 'NONE',  ( 12.00000000000000000, 5.563974596215566670, 1.734723475976807094E-15 ) ) ;
#7253 = CARTESIAN_POINT ( 'NONE',  ( -4.222908164277692222, 32.52819618069426610, 12.82270994545682186 ) ) ;
#7254 = CARTESIAN_POINT ( 'NONE',  ( -8.891200544363830713E-16, 37.67999999999999261, 13.50000000000000000 ) ) ;
#7255 = CARTESIAN_POINT ( 'NONE',  ( 13.49999999999999822, 62.28000000000000824, 4.386415899144236796 ) ) ;
#7256 = CIRCLE ( 'NONE', #3853, 13.50000000000000000 ) ;
#7257 = CARTESIAN_POINT ( 'NONE',  ( 13.50000000000000000, 83.43000000000000682, 1.653273178848926867E-15 ) ) ;
#7258 = CARTESIAN_POINT ( 'NONE',  ( 9.335235950531815854E-15, 58.17999999999999972, -13.50000000000000178 ) ) ;
#7259 = CARTESIAN_POINT ( 'NONE',  ( -4.357703367820035645, 38.52328190763838478, 12.77734288095807713 ) ) ;
#7260 = CARTESIAN_POINT ( 'NONE',  ( 5.801264985213661518, 36.96892180672517014, -12.19006904687155313 ) ) ;
#7261 = CARTESIAN_POINT ( 'NONE',  ( -13.50000000000000000, 69.93000000000000682, -3.306546357697853733E-15 ) ) ;
#7262 = LINE ( 'NONE', #12646, #2705 ) ;
#7263 = CARTESIAN_POINT ( 'NONE',  ( 11.56743521769684158, 63.17051234748981159, 6.960209698953964796 ) ) ;
#7264 = CARTESIAN_POINT ( 'NONE',  ( 8.112166317082673217, 41.98791513809585751, 10.79114295580683702 ) ) ;
#7265 = CARTESIAN_POINT ( 'NONE',  ( 8.998313441448996031, 48.83125608138507801, -10.07864022935939374 ) ) ;
#7266 = CARTESIAN_POINT ( 'NONE',  ( -11.76794919243112325, 19.08000000000001606, 3.823638476888994386 ) ) ;
#7267 = EDGE_CURVE ( 'NONE', #309, #6661, #4840, .T. ) ;
#7268 = ORIENTED_EDGE ( 'NONE', *, *, #8980, .F. ) ;
#7269 = CARTESIAN_POINT ( 'NONE',  ( 7.272992578804311492, 67.87999999999998124, -10.01041549318726886 ) ) ;
#7270 = CARTESIAN_POINT ( 'NONE',  ( 11.37499999999960565, -8.359374999999960920, 4.711679271994918317 ) ) ;
#7271 = CARTESIAN_POINT ( 'NONE',  ( -11.37499999999960387, -57.23437499999987921, -4.711679271994911211 ) ) ;
#7272 = VERTEX_POINT ( 'NONE', #12966 ) ;
#7273 = CARTESIAN_POINT ( 'NONE',  ( -0.01386867818632892685, 43.18049866634735423, -13.49999465302926716 ) ) ;
#7274 = CARTESIAN_POINT ( 'NONE',  ( 8.446640517145640834E-14, 43.67999999999999972, 13.50000000000000000 ) ) ;
#7275 = SHAPE_REPRESENTATION ( 'MAT-049', ( #15798, #16946, #7648, #5109, #13550 ), #5391 ) ;
#7276 = CARTESIAN_POINT ( 'NONE',  ( -10.92172942406178926, 2.629999999999993676, -7.935100905948389460 ) ) ;
#7277 = CARTESIAN_POINT ( 'NONE',  ( 13.16986379960055054, -18.73124999999995666, -13.16986379959834430 ) ) ;
#7278 = CARTESIAN_POINT ( 'NONE',  ( 8.606806894175420553, 66.01052269069948863, 10.40195802859246577 ) ) ;
#7279 = CARTESIAN_POINT ( 'NONE',  ( 6.123233995736766282E-16, 73.00000000000001421, 5.000000000000000000 ) ) ;
#7280 = CARTESIAN_POINT ( 'NONE',  ( -3.636496289402155746, 63.53000000000000114, 11.19198476289190936 ) ) ;
#7281 = CARTESIAN_POINT ( 'NONE',  ( -10.92172942406178926, 33.63000000000000256, -7.935100905948389460 ) ) ;
#7282 = CARTESIAN_POINT ( 'NONE',  ( 11.76794919243112325, 61.27999999999999403, 3.823638476888996607 ) ) ;
#7283 = CARTESIAN_POINT ( 'NONE',  ( -13.35791772474320815, 46.86141354909250367, -1.958702153931820567 ) ) ;
#7284 = CARTESIAN_POINT ( 'NONE',  ( 11.35334624979329909, 45.70351276252048933, -7.307357026597509631 ) ) ;
#7285 = CARTESIAN_POINT ( 'NONE',  ( 1.469576158976824144E-15, -28.00000000000000000, -12.00000000000000178 ) ) ;
#7286 = CARTESIAN_POINT ( 'NONE',  ( -25.42428528562849266, 5.918584287042170544, -5.441113646577749208 ) ) ;
#7287 = CARTESIAN_POINT ( 'NONE',  ( 11.25043742152392312, 30.71012671521651427, -7.461806818123373652 ) ) ;
#7288 = CARTESIAN_POINT ( 'NONE',  ( -13.43724082756498639, 55.88450770272648782, -1.312471336124251930 ) ) ;
#7289 = CARTESIAN_POINT ( 'NONE',  ( 0.000000000000000000, 80.93000000000000682, 0.000000000000000000 ) ) ;
#7290 = CARTESIAN_POINT ( 'NONE',  ( 9.155616606007495051, 33.03665467976623660, 9.920960544697097205 ) ) ;
#7291 = CARTESIAN_POINT ( 'NONE',  ( 0.000000000000000000, 73.00000000000001421, 0.000000000000000000 ) ) ;
#7292 = CARTESIAN_POINT ( 'NONE',  ( 10.31333816299139805, 39.76410056892473222, -8.711213421668183798 ) ) ;
#7293 = VERTEX_POINT ( 'NONE', #598 ) ;
#7294 = CARTESIAN_POINT ( 'NONE',  ( -10.96121799096760974, 62.22774600049994831, 7.881493374224405102 ) ) ;
#7295 = ORIENTED_EDGE ( 'NONE', *, *, #8281, .T. ) ;
#7296 = CARTESIAN_POINT ( 'NONE',  ( -13.27118709707405131, 40.84240854419702771, -2.487365594126258017 ) ) ;
#7297 = CARTESIAN_POINT ( 'NONE',  ( 2.621994543952811015E-15, 31.18000000000000682, -14.19474002721660355 ) ) ;
#7298 = CARTESIAN_POINT ( 'NONE',  ( -18.62499999999935341, -47.83437499999990195, -7.714727599200458030 ) ) ;
#7299 = CARTESIAN_POINT ( 'NONE',  ( 8.173436778830255989, 47.99018683713303091, 10.78145662369851898 ) ) ;
#7300 = CARTESIAN_POINT ( 'NONE',  ( 13.49999999999999822, 65.28000000000000114, 4.386415899144236796 ) ) ;
#7301 = CARTESIAN_POINT ( 'NONE',  ( -10.92172942406179104, 32.22999999999999687, 7.935100905948387684 ) ) ;
#7302 = CARTESIAN_POINT ( 'NONE',  ( -4.171729424061787483, 39.32999999999999829, -12.83926296998457417 ) ) ;
#7303 = AXIS2_PLACEMENT_3D ( 'NONE', #16403, #4305, #15063 ) ;
#7304 = CARTESIAN_POINT ( 'NONE',  ( -9.620510893913072792, 46.55969245225834641, -9.470785098964443094 ) ) ;
#7305 = PLANE ( 'NONE',  #16703 ) ;
#7306 = CARTESIAN_POINT ( 'NONE',  ( -8.043339635996304082, -65.59374999999981526, -8.043339635997652337 ) ) ;
#7307 = CARTESIAN_POINT ( 'NONE',  ( 10.81364905848734104, 54.12376407303845127, 8.082190041977272088 ) ) ;
#7308 = ORIENTED_EDGE ( 'NONE', *, *, #319, .F. ) ;
#7309 = CARTESIAN_POINT ( 'NONE',  ( -6.109331651355537574, 64.40329291578021298, -12.03877916920419366 ) ) ;
#7310 = EDGE_CURVE ( 'NONE', #16538, #10472, #3337, .T. ) ;
#7311 = ORIENTED_EDGE ( 'NONE', *, *, #13864, .F. ) ;
#7312 = CARTESIAN_POINT ( 'NONE',  ( 0.5902846111940708296, 67.15877554305052399, -13.50000000000000178 ) ) ;
#7313 = CARTESIAN_POINT ( 'NONE',  ( -5.644265419545289042, 34.38500592501070230, -12.26351404149298752 ) ) ;
#7314 = CARTESIAN_POINT ( 'NONE',  ( -4.711679271993004292, -21.85312499999995239, -11.37500000000039435 ) ) ;
#7315 = VECTOR ( 'NONE', #8095, 1000.000000000000000 ) ;
#7316 = CARTESIAN_POINT ( 'NONE',  ( 8.676621035646554958, 78.01381292210301410, 10.34245816167857690 ) ) ;
#7317 = CARTESIAN_POINT ( 'NONE',  ( -16.97418022790857961, 7.854708479871425730, 8.022689779262547560 ) ) ;
#7318 = CARTESIAN_POINT ( 'NONE',  ( 12.50000000000000000, 98.93000000000002103, 1.224646799147353059E-15 ) ) ;
#7319 = FACE_OUTER_BOUND ( 'NONE', #4264, .T. ) ;
#7320 = CARTESIAN_POINT ( 'NONE',  ( 11.41197208916220518, 72.16015570436597670, 7.212546593606687040 ) ) ;
#7321 = CARTESIAN_POINT ( 'NONE',  ( -11.76794919243112325, 30.93000000000001393, -2.602085213965210642E-15 ) ) ;
#7322 = CARTESIAN_POINT ( 'NONE',  ( 10.92172942406178926, 60.13000000000000256, 7.935100905948387684 ) ) ;
#7323 = CARTESIAN_POINT ( 'NONE',  ( -5.816118839772840055, 52.39170762701569828, -12.18289214338606818 ) ) ;
#7324 = CARTESIAN_POINT ( 'NONE',  ( -7.272992578804310604, 36.37999999999998835, 10.01041549318726709 ) ) ;
#7325 = CARTESIAN_POINT ( 'NONE',  ( 3.636496289402157078, -14.96999999999999709, -11.19198476289190936 ) ) ;
#7326 = CARTESIAN_POINT ( 'NONE',  ( 10.92172942406178926, 53.12999999999999545, 7.935100905948387684 ) ) ;
#7327 = CARTESIAN_POINT ( 'NONE',  ( 18.11515225121978290, 8.027996313748971602, 0.6918446750615231400 ) ) ;
#7328 = AXIS2_PLACEMENT_3D ( 'NONE', #10422, #607, #6445 ) ;
#7329 = CARTESIAN_POINT ( 'NONE',  ( 7.272992578804311492, -6.120000000000004547, -10.01041549318726709 ) ) ;
#7330 = CARTESIAN_POINT ( 'NONE',  ( 11.69227698284627337, 69.17914002359731285, 6.748504071555379902 ) ) ;
#7331 = CARTESIAN_POINT ( 'NONE',  ( 7.416407864998755706, 3.013974596215577950, -10.20780970022449807 ) ) ;
#7332 = CARTESIAN_POINT ( 'NONE',  ( 18.99999999999999289, 0.000000000000000000, 1.732050807568941586 ) ) ;
#7333 = CARTESIAN_POINT ( 'NONE',  ( 18.62500000000000000, -73.84999999999983800, 1.560692158462880521E-12 ) ) ;
#7334 = CARTESIAN_POINT ( 'NONE',  ( -13.35524205937507602, 73.86096575848492307, -1.971718875867300103 ) ) ;
#7335 = CARTESIAN_POINT ( 'NONE',  ( -2.392111896138028104, 76.26601152105787662, -13.28637674647000821 ) ) ;
#7336 = EDGE_CURVE ( 'NONE', #13170, #14800, #11264, .T. ) ;
#7337 = CARTESIAN_POINT ( 'NONE',  ( -4.441163314466836098, 79.33975151259672032, -12.74869167447762308 ) ) ;
#7338 = CARTESIAN_POINT ( 'NONE',  ( -7.379696451821980833E-14, 6.046025403784444308, -12.00000000000000000 ) ) ;
#7339 = CARTESIAN_POINT ( 'NONE',  ( -13.50000000000000000, 26.93000000000001037, -3.469446951953614189E-15 ) ) ;
#7340 = CARTESIAN_POINT ( 'NONE',  ( 9.520470885617715595, -3.869999999999998330, 6.917026985038135400 ) ) ;
#7341 = CARTESIAN_POINT ( 'NONE',  ( 9.520470885617715595, 37.12999999999999545, 6.917026985038134512 ) ) ;
#7342 = B_SPLINE_CURVE_WITH_KNOTS ( 'NONE', 3,
 ( #2765, #1197, #7932, #12245, #16030, #6609, #12157, #9266, #14701, #10582, #10750, #2591, #15943, #4025, #9440, #8021, #13389, #138 ),
 .UNSPECIFIED., .F., .F.,
 ( 4, 2, 2, 2, 2, 2, 2, 2, 4 ),
 ( 2.344180274388505696E-07, 0.0005273255548235158355, 0.001054416691619592837, 0.001581507828415669838, 0.002108598965211747056, 0.002635690102007827093, 0.003162781238803906696, 0.003689872375599986733, 0.004216963512396066337 ),
 .UNSPECIFIED. ) ;
#7343 = UNCERTAINTY_MEASURE_WITH_UNIT (LENGTH_MEASURE( 1.000000000000000082E-05 ), #8769, 'distance_accuracy_value', 'NONE');
#7344 = CARTESIAN_POINT ( 'NONE',  ( -12.50000000000000000, -18.00000000000000355, -9.000000000000001776 ) ) ;
#7345 = CARTESIAN_POINT ( 'NONE',  ( 7.999999999999904965, 7.773118517290098950, 17.32050807568881368 ) ) ;
#7346 = CARTESIAN_POINT ( 'NONE',  ( 5.918455295475054889, 74.89572671431407969, 12.13351137210443653 ) ) ;
#7347 = VECTOR ( 'NONE', #2255, 1000.000000000000000 ) ;
#7348 = CARTESIAN_POINT ( 'NONE',  ( 13.49791439481672839, 60.43900620806144275, -0.2626274307333924529 ) ) ;
#7349 = CARTESIAN_POINT ( 'NONE',  ( 0.000000000000000000, 0.000000000000000000, 0.000000000000000000 ) ) ;
#7350 = CARTESIAN_POINT ( 'NONE',  ( 4.171729424061789260, 82.82999999999999829, 12.83926296998457417 ) ) ;
#7351 = CARTESIAN_POINT ( 'NONE',  ( -2.420164038214338120, 58.26702013926823298, -13.28133895319109747 ) ) ;
#7352 = VECTOR ( 'NONE', #15592, 1000.000000000000000 ) ;
#7353 = CARTESIAN_POINT ( 'NONE',  ( -4.373507997709555895, 38.52270764513675516, 12.77194180747198615 ) ) ;
#7354 = CARTESIAN_POINT ( 'NONE',  ( 9.999999999999902300, 0.000000000000000000, 17.32050807568882789 ) ) ;
#7355 = DIRECTION ( 'NONE',  ( 1.000000000000000000, 8.673617379884039170E-17, -0.000000000000000000 ) ) ;
#7356 = DIRECTION ( 'NONE',  ( -1.000000000000000000, -0.000000000000000000, -0.000000000000000000 ) ) ;
#7357 = CARTESIAN_POINT ( 'NONE',  ( 9.628276390875990742, 63.06008494831254296, 9.462902099174160142 ) ) ;
#7358 = CARTESIAN_POINT ( 'NONE',  ( 5.447755521502024578, 41.87741670420104612, 12.35200281313600001 ) ) ;
#7359 = CARTESIAN_POINT ( 'NONE',  ( 11.05250497172135304, 48.72225972937487626, -7.756270235652836575 ) ) ;
#7360 = CARTESIAN_POINT ( 'NONE',  ( 11.76794919243112325, 17.42999999999999972, 1.734723475976807094E-15 ) ) ;
#7361 = ORIENTED_EDGE ( 'NONE', *, *, #13479, .F. ) ;
#7362 = CARTESIAN_POINT ( 'NONE',  ( 3.636496289402154414, 63.82999999999999829, 11.19198476289190936 ) ) ;
#7363 = CARTESIAN_POINT ( 'NONE',  ( -8.043339635996304082, -32.29374999999990337, -8.043339635997652337 ) ) ;
#7364 = CARTESIAN_POINT ( 'NONE',  ( -9.552639591052204498E-13, -29.13749999999993179, 11.37500000000000000 ) ) ;
#7365 = FACE_OUTER_BOUND ( 'NONE', #1626, .T. ) ;
#7366 = CARTESIAN_POINT ( 'NONE',  ( 0.7057993694291405662, 80.92999999999997840, -13.10211957505608638 ) ) ;
#7367 = CARTESIAN_POINT ( 'NONE',  ( -13.16986379959834252, -56.19374999999985931, -13.16986379960055054 ) ) ;
#7368 = CARTESIAN_POINT ( 'NONE',  ( 10.20702290661970579, 66.09018350808118214, 8.835545813414038108 ) ) ;
#7369 = CIRCLE ( 'NONE', #2247, 22.50000000000000355 ) ;
#7370 = CYLINDRICAL_SURFACE ( 'NONE', #4537, 12.00000000000000178 ) ;
#7371 = CARTESIAN_POINT ( 'NONE',  ( 11.76794919243112680, 46.57999999999999829, -3.823638476888993942 ) ) ;
#7372 = CARTESIAN_POINT ( 'NONE',  ( 13.50000000000000000, 32.42999999999999972, 1.653273178848926867E-15 ) ) ;
#7373 = CARTESIAN_POINT ( 'NONE',  ( 9.520470885617717371, 58.73000000000000398, -6.917026985038131848 ) ) ;
#7374 = CARTESIAN_POINT ( 'NONE',  ( -13.42542795491608310, 46.98152504557900500, 1.474995282428532395 ) ) ;
#7375 = EDGE_CURVE ( 'NONE', #14459, #9696, #4363, .T. ) ;
#7376 = CARTESIAN_POINT ( 'NONE',  ( 11.92132692379593628, 45.66421514304773410, -6.337276081506336922 ) ) ;
#7377 = CARTESIAN_POINT ( 'NONE',  ( 6.262084934075358156, 69.95073729743167235, -11.96369458021704446 ) ) ;
#7378 = DIRECTION ( 'NONE',  ( 0.000000000000000000, 0.000000000000000000, -1.000000000000000000 ) ) ;
#7379 = CARTESIAN_POINT ( 'NONE',  ( 5.816537829104611923, 30.96824124766034103, -12.18269343281530048 ) ) ;
#7380 = CARTESIAN_POINT ( 'NONE',  ( -12.17509508611693292, 55.71589168976755957, -5.832679525784597807 ) ) ;
#7381 = CARTESIAN_POINT ( 'NONE',  ( -2.463123716452229051, 50.59134218680501505, 13.27377621386196260 ) ) ;
#7382 = DIRECTION ( 'NONE',  ( 0.000000000000000000, 0.000000000000000000, -1.000000000000000000 ) ) ;
#7383 = CARTESIAN_POINT ( 'NONE',  ( 4.662704016964861253, 43.01217040675273040, -12.67144116224080719 ) ) ;
#7384 = CARTESIAN_POINT ( 'NONE',  ( 9.961534293312238830, 39.78284768016499839, -9.113236095871735998 ) ) ;
#7385 = EDGE_LOOP ( 'NONE', ( #8732, #10405, #14565, #11853 ) ) ;
#7386 = CARTESIAN_POINT ( 'NONE',  ( -13.45835841592290016, 61.96676735775977107, 1.061614036730301525 ) ) ;
#7387 =( BOUNDED_CURVE ( )  B_SPLINE_CURVE ( 2, ( #1750, #8584, #520, #11307, #15347, #17118, #2170, #12974, #693, #16945, #6267, #12808, #10170 ),
 .UNSPECIFIED., .F., .F. ) 
 B_SPLINE_CURVE_WITH_KNOTS ( ( 3, 2, 2, 2, 2, 2, 3 ),
 ( 0.4583333333333333148, 0.4611111111111111382, 0.4666666666666666741, 0.4722222222222222099, 0.4777777777777778012, 0.4833333333333333370, 0.4861111111111111049 ),
 .UNSPECIFIED. ) 
 CURVE ( )  GEOMETRIC_REPRESENTATION_ITEM ( )  RATIONAL_B_SPLINE_CURVE ( ( 0.9755282581475768211, 0.9755282581475765991, 1.000000000000000000, 0.9510565162951535312, 1.000000000000000000, 0.9510565162951535312, 1.000000000000000000, 0.9510565162951535312, 1.000000000000000000, 0.9510565162951535312, 1.000000000000000000, 0.9755282581475768211, 0.9755282581475768211 ) ) 
 REPRESENTATION_ITEM ( '' )  );
#7388 = ORIENTED_EDGE ( 'NONE', *, *, #13084, .F. ) ;
#7389 = VERTEX_POINT ( 'NONE', #2248 ) ;
#7390 = CARTESIAN_POINT ( 'NONE',  ( 10.92172942406179104, 30.73000000000000753, -7.935100905948385908 ) ) ;
#7391 = CARTESIAN_POINT ( 'NONE',  ( 1.561832610794586740E-12, -94.66249999999980957, -18.62500000000000000 ) ) ;
#7392 = CARTESIAN_POINT ( 'NONE',  ( 4.964042911967482929, 58.00092663269024484, -12.55448936394250303 ) ) ;
#7393 = CARTESIAN_POINT ( 'NONE',  ( -7.272992578804307939, 77.48000000000000398, -10.01041549318726886 ) ) ;
#7394 = CARTESIAN_POINT ( 'NONE',  ( -4.171729424061787483, 42.32999999999999829, -12.83926296998457417 ) ) ;
#7395 = ADVANCED_FACE ( 'NONE', ( #7676 ), #13055, .F. ) ;
#7396 = CARTESIAN_POINT ( 'NONE',  ( -6.293574425437782338, 46.41065374424994161, -11.94324194161466934 ) ) ;
#7397 = CARTESIAN_POINT ( 'NONE',  ( 17.32050807568873552, 0.000000000000000000, 8.000000000000085265 ) ) ;
#7398 = CARTESIAN_POINT ( 'NONE',  ( -8.043339635996304082, -15.64374999999994387, -8.043339635997652337 ) ) ;
#7399 = CARTESIAN_POINT ( 'NONE',  ( 4.934664456648047981, 53.85797222871626388, 12.56582013419890664 ) ) ;
#7400 = ORIENTED_EDGE ( 'NONE', *, *, #8549, .T. ) ;
#7401 = CARTESIAN_POINT ( 'NONE',  ( 12.50000000000000000, -18.00000000000000355, 8.999999999999998224 ) ) ;
#7402 = EDGE_LOOP ( 'NONE', ( #12126, #6687, #3492, #6620 ) ) ;
#7403 = AXIS2_PLACEMENT_3D ( 'NONE', #7689, #15698, #14636 ) ;
#7404 = DIRECTION ( 'NONE',  ( 6.313931023057711093E-15, -0.000000000000000000, -1.000000000000000000 ) ) ;
#7405 = CARTESIAN_POINT ( 'NONE',  ( -6.892083252854373399, 34.43494372278320981, -11.62035706217954889 ) ) ;
#7406 = CARTESIAN_POINT ( 'NONE',  ( -8.043339635997652337, -34.30624999999993463, 8.043339635996300530 ) ) ;
#7407 = CARTESIAN_POINT ( 'NONE',  ( 7.127680621519133730, 77.94494083559413866, 11.47363209226457492 ) ) ;
#7408 = CARTESIAN_POINT ( 'NONE',  ( -15.31970530204994674, 8.007293614239923585, 9.835827272001230526 ) ) ;
#7409 = CARTESIAN_POINT ( 'NONE',  ( 16.03540712409202484, 8.027799080943070820, 8.457499700851130342 ) ) ;
#7410 = DIRECTION ( 'NONE',  ( 0.000000000000000000, 1.000000000000000000, 0.000000000000000000 ) ) ;
#7411 = CARTESIAN_POINT ( 'NONE',  ( 12.99914974011805668, 72.56016066728088276, -3.643509121896943093 ) ) ;
#7412 = CARTESIAN_POINT ( 'NONE',  ( 11.76794919243112680, 26.57999999999999829, -3.823638476888993942 ) ) ;
#7413 = CARTESIAN_POINT ( 'NONE',  ( 4.171729424061791924, 64.03000000000000114, -12.83926296998457239 ) ) ;
#7414 = CARTESIAN_POINT ( 'NONE',  ( -2.186818166953001796, 52.25862599162246624, -13.32198785724745527 ) ) ;
#7415 = EDGE_CURVE ( 'NONE', #309, #2603, #3923, .T. ) ;
#7416 = CARTESIAN_POINT ( 'NONE',  ( 11.76794919243112325, 34.42999999999999261, 1.441158131103945434E-15 ) ) ;
#7417 = CARTESIAN_POINT ( 'NONE',  ( -7.409984580736203970E-16, -16.32000000000000028, 12.37355403259654985 ) ) ;
#7418 = CARTESIAN_POINT ( 'NONE',  ( 4.171729424061791924, 54.03000000000000114, -12.83926296998457239 ) ) ;
#7419 = CIRCLE ( 'NONE', #16428, 26.00000000000000355 ) ;
#7420 = CARTESIAN_POINT ( 'NONE',  ( 0.000000000000000000, 5.918584287042170544, 0.000000000000000000 ) ) ;
#7421 = CARTESIAN_POINT ( 'NONE',  ( -11.76794919243112325, -1.920000000000006590, 3.823638476888994386 ) ) ;
#7422 = CARTESIAN_POINT ( 'NONE',  ( -4.433484632589104635, 68.52052440024017699, 12.75127848232592775 ) ) ;
#7423 = CARTESIAN_POINT ( 'NONE',  ( 13.16986379960055054, -18.73124999999995666, -13.16986379959834430 ) ) ;
#7424 = CARTESIAN_POINT ( 'NONE',  ( -2.970370385949441694, 7.170662809914418290, 21.14483242576212163 ) ) ;
#7425 = CARTESIAN_POINT ( 'NONE',  ( -7.714727599200466912, -51.99687499999990337, 18.62499999999935341 ) ) ;
#7426 = CARTESIAN_POINT ( 'NONE',  ( -13.47341305627475272, 73.90037531866931886, -0.8597925056511297459 ) ) ;
#7427 = CARTESIAN_POINT ( 'NONE',  ( -7.413775151259285323, 76.45717531281798074, -11.28405773006812574 ) ) ;
#7428 = CARTESIAN_POINT ( 'NONE',  ( 10.35194220012931154, 7.925732005390763391, -15.34409809138587022 ) ) ;
#7429 = CARTESIAN_POINT ( 'NONE',  ( 10.00000000000135891, 7.983052681821872554, -15.32050807568352191 ) ) ;
#7430 = CARTESIAN_POINT ( 'NONE',  ( 10.92172942406178926, 25.13000000000001322, 7.935100905948385908 ) ) ;
#7431 = CARTESIAN_POINT ( 'NONE',  ( 7.272992578804308828, 33.97999999999999687, 10.01041549318726886 ) ) ;
#7432 = DIRECTION ( 'NONE',  ( -0.000000000000000000, -1.000000000000000000, -0.000000000000000000 ) ) ;
#7433 = AXIS2_PLACEMENT_3D ( 'NONE', #7175, #1766, #8685 ) ;
#7434 = CARTESIAN_POINT ( 'NONE',  ( -5.829253055094191005, 32.46794701112467862, 12.18592114757813327 ) ) ;
#7435 = CARTESIAN_POINT ( 'NONE',  ( 1.327664892297638843, 74.72773790534441218, 13.43455645011153621 ) ) ;
#7436 = DIRECTION ( 'NONE',  ( -0.000000000000000000, -1.000000000000000000, -0.000000000000000000 ) ) ;
#7437 = CARTESIAN_POINT ( 'NONE',  ( -13.50000000000000000, 78.93000000000000682, -3.306546357697853733E-15 ) ) ;
#7438 = ADVANCED_FACE ( 'NONE', ( #11000, #4276 ), #11089, .F. ) ;
#7439 = CARTESIAN_POINT ( 'NONE',  ( 11.63962625337223145, 51.68454806329603457, -6.839222346739858516 ) ) ;
#7440 = CARTESIAN_POINT ( 'NONE',  ( -12.73620748938531833, 38.09169207387569855, 4.479728807359646403 ) ) ;
#7441 = AXIS2_PLACEMENT_3D ( 'NONE', #1405, #6821, #3078 ) ;
#7442 = CARTESIAN_POINT ( 'NONE',  ( 11.22854147624287435, 36.71152521474294872, -7.494658285005058040 ) ) ;
#7443 = CARTESIAN_POINT ( 'NONE',  ( -11.37500000000039613, -59.31562499999985505, 4.711679271993002516 ) ) ;
#7444 = FACE_OUTER_BOUND ( 'NONE', #13728, .T. ) ;
#7445 = DIRECTION ( 'NONE',  ( -0.5000000000000041078, 0.000000000000000000, 0.8660254037844363761 ) ) ;
#7446 = CARTESIAN_POINT ( 'NONE',  ( 0.1518789328228659086, 62.68546100971695978, 13.49937261551957590 ) ) ;
#7447 = FACE_OUTER_BOUND ( 'NONE', #3302, .T. ) ;
#7448 = CARTESIAN_POINT ( 'NONE',  ( 13.49806724646292899, 48.45090782768691895, -0.6033653513361341147 ) ) ;
#7449 = CARTESIAN_POINT ( 'NONE',  ( 7.272992578804308828, 13.98000000000000220, 10.01041549318726709 ) ) ;
#7450 = ORIENTED_EDGE ( 'NONE', *, *, #10587, .F. ) ;
#7451 = CARTESIAN_POINT ( 'NONE',  ( -7.272992578804307939, 68.48000000000000398, -10.01041549318727064 ) ) ;
#7452 = CARTESIAN_POINT ( 'NONE',  ( 11.37500000000039613, -10.44062499999995453, -4.711679271993004292 ) ) ;
#7453 = CARTESIAN_POINT ( 'NONE',  ( 11.37500000000000000, -33.29999999999991900, 9.531744055041752924E-13 ) ) ;
#7454 = CARTESIAN_POINT ( 'NONE',  ( -10.92172942406178926, 1.629999999999992566, -7.935100905948389460 ) ) ;
#7455 = CARTESIAN_POINT ( 'NONE',  ( -0.02772103388578331384, 43.18099674618451189, -13.49997331539339562 ) ) ;
#7456 = CARTESIAN_POINT ( 'NONE',  ( 0.7664276751979015589, 76.15244233678546948, -13.47830342854411079 ) ) ;
#7457 = CARTESIAN_POINT ( 'NONE',  ( -1.564113515457998572E-12, -45.78749999999988773, 18.62500000000000000 ) ) ;
#7458 = CARTESIAN_POINT ( 'NONE',  ( 6.534285954687437226, 65.92034066636635714, 11.81874242131197050 ) ) ;
#7459 = CARTESIAN_POINT ( 'NONE',  ( -10.92172942406178926, 82.62999999999999545, -7.935100905948389460 ) ) ;
#7460 = CARTESIAN_POINT ( 'NONE',  ( 7.272992578804308828, 45.98000000000000398, 10.01041549318726709 ) ) ;
#7461 = ADVANCED_FACE ( 'NONE', ( #7031 ), #2750, .T. ) ;
#7462 = CARTESIAN_POINT ( 'NONE',  ( -12.41832812777009920, 59.12332451315333515, 5.299458117618179642 ) ) ;
#7463 = CARTESIAN_POINT ( 'NONE',  ( 13.04194034339959885, 45.55439597745233726, -3.489029769191362096 ) ) ;
#7464 = CARTESIAN_POINT ( 'NONE',  ( 10.10108856181172143, 69.77545969696819839, -8.956536834962969706 ) ) ;
#7465 = PRESENTATION_STYLE_ASSIGNMENT (( #6142 ) ) ;
#7466 = CARTESIAN_POINT ( 'NONE',  ( 12.67585016484028948, 30.59854293864694696, -4.663455345598352508 ) ) ;
#7467 = CARTESIAN_POINT ( 'NONE',  ( -13.50529826739625783, 55.92983664685408485, 2.178437852371490542E-05 ) ) ;
#7468 = CARTESIAN_POINT ( 'NONE',  ( 4.171729424061791924, 54.03000000000000114, -12.83926296998457239 ) ) ;
#7469 = CARTESIAN_POINT ( 'NONE',  ( 9.829015088374500664, 63.78966567892446449, -9.254229041624375540 ) ) ;
#7470 = CARTESIAN_POINT ( 'NONE',  ( 1.486569204522005805, 43.12668836574830067, -13.41992218948748317 ) ) ;
#7471 = CARTESIAN_POINT ( 'NONE',  ( 9.048820653867387875, 39.82882913570732342, -10.03219236511709056 ) ) ;
#7472 = EDGE_LOOP ( 'NONE', ( #14520, #6270, #6536, #6470 ) ) ;
#7473 = CARTESIAN_POINT ( 'NONE',  ( -11.09391357339225337, 62.21979212502633771, 7.692540733092653404 ) ) ;
#7474 = ORIENTED_EDGE ( 'NONE', *, *, #4672, .F. ) ;
#7475 = EDGE_LOOP ( 'NONE', ( #3931, #4286, #8907, #8947 ) ) ;
#7476 = CARTESIAN_POINT ( 'NONE',  ( -13.49999999999999822, 32.08000000000001251, 4.386415899144235908 ) ) ;
#7477 = CARTESIAN_POINT ( 'NONE',  ( -18.62499999999934985, -23.93437499999993889, -7.714727599200458918 ) ) ;
#7478 = CARTESIAN_POINT ( 'NONE',  ( 13.07592573315582385, 48.31048427460937944, 3.357180248748443674 ) ) ;
#7479 = CARTESIAN_POINT ( 'NONE',  ( 10.48295876490647593, 57.75483760623548335, -8.506347226123828875 ) ) ;
#7480 = CARTESIAN_POINT ( 'NONE',  ( 10.57584348060936286, 78.74972999058537937, -8.393457333304862544 ) ) ;
#7481 = CARTESIAN_POINT ( 'NONE',  ( 11.76794919243112325, 79.28000000000001535, 3.823638476888996607 ) ) ;
#7482 = CARTESIAN_POINT ( 'NONE',  ( 7.329991333342587012, -1.736202706843530252E-17, -9.501117147637041072 ) ) ;
#7483 = CARTESIAN_POINT ( 'NONE',  ( -1.539363535742758637, 7.854661454367255935, 18.71158131929041701 ) ) ;
#7484 = CARTESIAN_POINT ( 'NONE',  ( -0.2663380794371886795, 67.18957635750793145, -13.49772504475413193 ) ) ;
#7485 = CARTESIAN_POINT ( 'NONE',  ( 4.711679271994911211, -45.82187499999987779, -11.37499999999960743 ) ) ;
#7486 =( BOUNDED_SURFACE ( )  B_SPLINE_SURFACE ( 1, 2, ( 
 ( #13679, #15174, #12370, #11227, #12550, #16513, #16601, #1577, #4420, #4594, #3250, #4328, #9736, #8412, #1664, #12463, #3074, #8500, #436, #13850, #1753, #5844, #11310, #14031, #4508, #15262, #1919, #3160, #1832, #7249, #12282, #177, #11489, #15438, #4767, #10338, #5025, #11573, #6269, #695, #7339, #12893, #8928, #12722, #16774, #2172, #4682, #8762, #609, #3599, #7511, #2004, #7430, #10172, #11656, #15521, #2257, #8848, #7685, #16948, #4849, #7598, #12976, #859, #946, #6359, #17120, #15784, #3693, #10763, #10848, #2429, #6619, #2691, #6791, #13400, #11915, #6703, #5296, #17463, #7860, #11999, #6447, #14631, #12171, #4127, #2516, #2346, #62, #13235, #5120, #7778, #15874, #9193, #17293, #5206, #10596, #15958, #9279, #7945, #16664, #12787, #4658, #673, #11550, #11465, #16841, #10149, #6777, #14965, #10815, #16273, #16010, #16178, #9678, #15028, #9333, #8000, #14682, #2570, #1338, #13368, #4089, #114, #9505, #12052, #6844, #5611, #1607, #1257, #10903, #16361, #14766, #6934, #2833, #6669, #14851, #16094, #17430, #9418, #9591, #2921, #2744, #4179, #5343, #7023, #5426, #13538, #5261, #3916, #1427, #10729, #4002, #17349, #8264, #6755, #10647, #2658, #8088, #14942, #13452, #13624, #12134, #1517, #23, #8174, #12221, #5520, #12312, #205, #10993, #4268, #8351, #13708, #3282, #3608, #12491, #11252, #8698, #376, #15701, #4621, #13878, #5782, #12659, #13793, #7107, #15111, #14059, #11167, #290, #16631, #3009, #1779, #16543, #4534, #9020, #11080, #1862, #8439, #16453, #7188, #7276, #9941, #15290, #1692, #4356, #3191, #14376, #4449, #8613, #9765, #5873, #9856, #13965, #7605, #548, #5699, #15202, #3102, #866, #8530, #5958, #12577, #465, #11338, #2264, #6276, #16715, #10027, #12402, #15375, #2179, #12983, #11664, #17040, #4945, #10346, #6453, #9112, #3787, #5213, #3958, #5303, #11839, #1296, #4044, #10516, #17388, #10685, #6367, #5384, #9458, #12088, #8040, #15967, #6627, #5126, #9371, #13242, #6710, #3699, #16132, #13157, #2353, #9200, #17471, #14551, #17215, #10769, #1131, #6542, #14721, #1043, #13407, #17301, #9286, #13070, #14464, #2525, #7785, #2609, #7954, #16051, #13324, #1216, #11750, #12006, #14806, #7691, #955, #17126, #5034, #10433, #15792, #12533, #69, #1383, #16495, #8220, #14984, #2789, #11121, #12355, #5826, #9811, #4221, #9899, #8484, #8309, #5740, #4134, #13664, #249, #12264, #16584, #161, #4400, #1559, #2699, #12446, #1648, #8128, #1473, #16315, #6800, #2965, #5474, #7064, #5566, #12178, #10855, #4489, #331, #16222, #15157, #9546, #3056, #14895, #13581, #9635, #6891, #10948, #8395, #2876, #5654, #6980, #11036, #13835, #11210, #16408, #4309, #1735, #9721, #13749 ),
 ( #419, #7148, #5914, #1904, #3330, #3419, #4751, #3236, #7499, #4837, #14011, #10157, #15507, #8569, #11558, #10240, #768, #2074, #8745, #6092, #7321, #8833, #11385, #12879, #506, #16934, #9985, #16672, #8656, #6176, #12705, #15333, #15594, #592, #6003, #14190, #16758, #15246, #4665, #10072, #13922, #11293, #15423, #4578, #3144, #14102, #1816, #16849, #1987, #7412, #12794, #680, #11472, #7230, #12618, #4553, #4467, #9872, #1443, #8280, #6861, #3119, #6951, #8368, #222, #13896, #9783, #5536, #481, #15043, #11009, #16380, #7041, #4285, #9695, #12419, #15130, #2939, #3027, #8457, #7123, #8032, #14884, #14711, #3947, #15777, #3776, #1119, #3688, #5292, #13145, #9361, #2422, #1033, #17459, #15869, #14454, #9274, #11827, #5202, #14537, #3860, #13484, #2341, #10674, #5114, #7856, #10592, #9447, #16039, #13231, #2599, #2512, #8028, #14627, #1205, #1285, #5372, #4033, #12166, #14795, #5020, #2687, #8118, #1548, #11111, #3224, #13998, #8731, #2063, #12101, #5486, #13255, #15979, #14563, #9300, #1142, #4145, #6723, #6553, #8055, #5227, #9470, #5398, #14734, #2712, #11933, #2622, #12279, #10529, #17313, #10612, #3882, #14650, #17399, #2538, #17483, #10782, #16147, #7966, #8141, #15891, #16065, #1396, #6812, #82, #2304, #7908, #3827, #11702, #9155, #3650, #13023, #14416, #10559, #10640, #5078, #17254, #10386, #14677, #15833, #7826, #3560, #14330, #13197, #2219, #7646, #15650, #14595, #17168, #905, #6316, #8974, #6582, #15740, #5253, #9063, #16004, #17079, #7732, #1083, #13108, #2390, #13283, #3738, #15918, #11791, #6496, #3910, #4984, #11879, #1171, #995, #5167, #6408, #9242, #2475, #11963, #17342, #9327, #11216, #1994, #6099, #9905, #427, #13928, #15341, #3338, #4673, #15252, #686, #10164, #8577, #10078, #15429, #15165, #11480, #15512, #16855, #7421, #3241, #6011, #1822, #8753, #5920, #4758, #12540, #3424, #16590, #4498, #3151, #4408, #7238, #12624, #9818, #16678, #512, #3063, #11301, #8490, #4585, #9993, #1743, #8664, #14021, #1911, #13841, #7329, #7155, #5833, #12712, #16765, #599, #11393, #10683, #158, #14893, #12262, #6798, #67, #1471, #2523, #15965, #16220, #12004, #1294, #17386, #4132, #5382, #5564, #9544, #2607, #16313, #2787, #12086, #5472, #13322, #17469, #16130, #16049, #17299, #4041, #7951, #8126, #1214, #6625, #5301, #9369, #9456, #1381, #3956, #8038, #12176, #14804, #2697, #13493, #8218, #13579, #8661, #15337, #4669, #4754, #1908, #3335, #14017, #8749, #7325, #14107, #683, #1991, #12709, #6007, #11390, #6096, #16762, #7417, #12799, #11476, #16852, #9990, #12537, #15161, #15070, #11041, #12450, #3060, #8399, #335, #5744, #1738, #11127, #424, #16501, #16412, #4405 ) ),
 .UNSPECIFIED., .F., .F., .F. ) 
 B_SPLINE_SURFACE_WITH_KNOTS ( ( 2, 2 ),
 ( 3, 2, 2, 2, 2, 2, 2, 2, 2, 2, 2, 2, 2, 2, 2, 2, 2, 2, 2, 2, 2, 2, 2, 2, 2, 2, 2, 2, 2, 2, 2, 2, 2, 2, 2, 2, 2, 2, 2, 2, 2, 2, 2, 2, 2, 2, 2, 2, 2, 2, 2, 2, 2, 2, 2, 2, 2, 2, 2, 2, 2, 2, 2, 2, 2, 2, 2, 2, 2, 2, 2, 2, 2, 2, 2, 2, 2, 2, 2, 2, 2, 2, 2, 2, 2, 2, 2, 2, 2, 2, 2, 2, 2, 2, 2, 2, 2, 2, 2, 2, 2, 2, 2, 2, 2, 2, 2, 2, 2, 2, 2, 2, 2, 2, 2, 2, 2, 2, 2, 2, 2, 2, 2, 2, 2, 2, 2, 2, 2, 2, 2, 2, 2, 2, 2, 2, 2, 2, 2, 2, 2, 2, 2, 2, 2, 2, 2, 2, 2, 2, 2, 2, 2, 2, 2, 2, 2, 2, 2, 2, 2, 2, 2, 2, 2, 2, 2, 2, 2, 2, 2, 2, 2, 2, 2, 2, 2, 3 ),
 ( 0.000000000000000000, 1.000000000000000000 ),
 ( 0.000000000000000000, 0.005555555555555555768, 0.01111111111111111154, 0.01666666666666666644, 0.02222222222222222307, 0.02777777777777777624, 0.03333333333333333287, 0.03888888888888888951, 0.04444444444444444614, 0.05000000000000000278, 0.05555555555555555247, 0.06111111111111110911, 0.06666666666666666574, 0.07222222222222221544, 0.07777777777777777901, 0.08333333333333332871, 0.08888888888888889228, 0.09444444444444444198, 0.1000000000000000056, 0.1055555555555555552, 0.1111111111111111049, 0.1166666666666666685, 0.1222222222222222182, 0.1277777777777777679, 0.1333333333333333315, 0.1388888888888888951, 0.1444444444444444309, 0.1499999999999999944, 0.1555555555555555580, 0.1611111111111111216, 0.1666666666666666574, 0.1722222222222222210, 0.1777777777777777846, 0.1833333333333333204, 0.1888888888888888840, 0.1944444444444444475, 0.2000000000000000111, 0.2055555555555555469, 0.2111111111111111105, 0.2166666666666666741, 0.2222222222222222099, 0.2277777777777777735, 0.2333333333333333370, 0.2388888888888889006, 0.2444444444444444364, 0.2500000000000000000, 0.2555555555555555358, 0.2611111111111111271, 0.2666666666666666630, 0.2722222222222221988, 0.2777777777777777901, 0.2833333333333333259, 0.2888888888888888618, 0.2944444444444444531, 0.2999999999999999889, 0.3055555555555555802, 0.3111111111111111160, 0.3166666666666666519, 0.3222222222222222432, 0.3277777777777777790, 0.3333333333333333148, 0.3388888888888889062, 0.3444444444444444420, 0.3499999999999999778, 0.3555555555555555691, 0.3611111111111111049, 0.3666666666666666408, 0.3722222222222222321, 0.3777777777777777679, 0.3833333333333333592, 0.3888888888888888951, 0.3944444444444444309, 0.4000000000000000222, 0.4055555555555555580, 0.4111111111111110938, 0.4166666666666666852, 0.4222222222222222210, 0.4277777777777777568, 0.4333333333333333481, 0.4388888888888888840, 0.4444444444444444198, 0.4500000000000000111, 0.4555555555555555469, 0.4611111111111111382, 0.4666666666666666741, 0.4722222222222222099, 0.4777777777777778012, 0.4833333333333333370, 0.4888888888888888729, 0.4944444444444444642, 0.5000000000000000000, 0.5055555555555555358, 0.5111111111111110716, 0.5166666666666667185, 0.5222222222222222543, 0.5277777777777777901, 0.5333333333333333259, 0.5388888888888888618, 0.5444444444444443976, 0.5500000000000000444, 0.5555555555555555802, 0.5611111111111111160, 0.5666666666666666519, 0.5722222222222221877, 0.5777777777777777235, 0.5833333333333333703, 0.5888888888888889062, 0.5944444444444444420, 0.5999999999999999778, 0.6055555555555555136, 0.6111111111111111605, 0.6166666666666666963, 0.6222222222222222321, 0.6277777777777777679, 0.6333333333333333037, 0.6388888888888888395, 0.6444444444444444864, 0.6500000000000000222, 0.6555555555555555580, 0.6611111111111110938, 0.6666666666666666297, 0.6722222222222222765, 0.6777777777777778123, 0.6833333333333333481, 0.6888888888888888840, 0.6944444444444444198, 0.6999999999999999556, 0.7055555555555556024, 0.7111111111111111382, 0.7166666666666666741, 0.7222222222222222099, 0.7277777777777777457, 0.7333333333333332815, 0.7388888888888889284, 0.7444444444444444642, 0.7500000000000000000, 0.7555555555555555358, 0.7611111111111110716, 0.7666666666666667185, 0.7722222222222222543, 0.7777777777777777901, 0.7833333333333333259, 0.7888888888888888618, 0.7944444444444443976, 0.8000000000000000444, 0.8055555555555555802, 0.8111111111111111160, 0.8166666666666666519, 0.8222222222222221877, 0.8277777777777777235, 0.8333333333333333703, 0.8388888888888889062, 0.8444444444444444420, 0.8499999999999999778, 0.8555555555555555136, 0.8611111111111111605, 0.8666666666666666963, 0.8722222222222222321, 0.8777777777777777679, 0.8833333333333333037, 0.8888888888888888395, 0.8944444444444444864, 0.9000000000000000222, 0.9055555555555555580, 0.9111111111111110938, 0.9166666666666666297, 0.9222222222222222765, 0.9277777777777778123, 0.9333333333333333481, 0.9388888888888888840, 0.9444444444444444198, 0.9499999999999999556, 0.9555555555555556024, 0.9611111111111111382, 0.9666666666666666741, 0.9722222222222222099, 0.9777777777777777457, 0.9814746806989694816 ),
 .UNSPECIFIED. ) 
 GEOMETRIC_REPRESENTATION_ITEM ( )  RATIONAL_B_SPLINE_SURFACE ( (
 ( 1.000000000000000000, 0.9510565162951535312, 1.000000000000000000, 0.9510565162951535312, 1.000000000000000000, 0.9510565162951535312, 1.000000000000000000, 0.9510565162951535312, 1.000000000000000000, 0.9510565162951535312, 1.000000000000000000, 0.9510565162951535312, 1.000000000000000000, 0.9510565162951535312, 1.000000000000000000, 0.9510565162951535312, 1.000000000000000000, 0.9510565162951535312, 1.000000000000000000, 0.9510565162951535312, 1.000000000000000000, 0.9510565162951535312, 1.000000000000000000, 0.9510565162951535312, 1.000000000000000000, 0.9510565162951535312, 1.000000000000000000, 0.9510565162951535312, 1.000000000000000000, 0.9510565162951535312, 1.000000000000000000, 0.9510565162951535312, 1.000000000000000000, 0.9510565162951535312, 1.000000000000000000, 0.9510565162951535312, 1.000000000000000000, 0.9510565162951535312, 1.000000000000000000, 0.9510565162951535312, 1.000000000000000000, 0.9510565162951535312, 1.000000000000000000, 0.9510565162951535312, 1.000000000000000000, 0.9510565162951535312, 1.000000000000000000, 0.9510565162951535312, 1.000000000000000000, 0.9510565162951535312, 1.000000000000000000, 0.9510565162951535312, 1.000000000000000000, 0.9510565162951535312, 1.000000000000000000, 0.9510565162951535312, 1.000000000000000000, 0.9510565162951535312, 1.000000000000000000, 0.9510565162951535312, 1.000000000000000000, 0.9510565162951535312, 1.000000000000000000, 0.9510565162951535312, 1.000000000000000000, 0.9510565162951535312, 1.000000000000000000, 0.9510565162951535312, 1.000000000000000000, 0.9510565162951535312, 1.000000000000000000, 0.9510565162951535312, 1.000000000000000000, 0.9510565162951535312, 1.000000000000000000, 0.9510565162951535312, 1.000000000000000000, 0.9510565162951535312, 1.000000000000000000, 0.9510565162951535312, 1.000000000000000000, 0.9510565162951535312, 1.000000000000000000, 0.9510565162951535312, 1.000000000000000000, 0.9510565162951535312, 1.000000000000000000, 0.9510565162951535312, 1.000000000000000000, 0.9510565162951535312, 1.000000000000000000, 0.9510565162951535312, 1.000000000000000000, 0.9510565162951535312, 1.000000000000000000, 0.9510565162951535312, 1.000000000000000000, 0.9510565162951535312, 1.000000000000000000, 0.9510565162951535312, 1.000000000000000000, 0.9510565162951535312, 1.000000000000000000, 0.9510565162951535312, 1.000000000000000000, 0.9510565162951535312, 1.000000000000000000, 0.9510565162951535312, 1.000000000000000000, 0.9510565162951535312, 1.000000000000000000, 0.9510565162951535312, 1.000000000000000000, 0.9510565162951535312, 1.000000000000000000, 0.9510565162951535312, 1.000000000000000000, 0.9510565162951535312, 1.000000000000000000, 0.9510565162951535312, 1.000000000000000000, 0.9510565162951535312, 1.000000000000000000, 0.9510565162951535312, 1.000000000000000000, 0.9510565162951535312, 1.000000000000000000, 0.9510565162951535312, 1.000000000000000000, 0.9510565162951535312, 1.000000000000000000, 0.9510565162951535312, 1.000000000000000000, 0.9510565162951535312, 1.000000000000000000, 0.9510565162951535312, 1.000000000000000000, 0.9510565162951535312, 1.000000000000000000, 0.9510565162951535312, 1.000000000000000000, 0.9510565162951535312, 1.000000000000000000, 0.9510565162951535312, 1.000000000000000000, 0.9510565162951535312, 1.000000000000000000, 0.9510565162951535312, 1.000000000000000000, 0.9510565162951535312, 1.000000000000000000, 0.9510565162951535312, 1.000000000000000000, 0.9510565162951535312, 1.000000000000000000, 0.9510565162951535312, 1.000000000000000000, 0.9510565162951535312, 1.000000000000000000, 0.9510565162951535312, 1.000000000000000000, 0.9510565162951535312, 1.000000000000000000, 0.9510565162951535312, 1.000000000000000000, 0.9510565162951535312, 1.000000000000000000, 0.9510565162951535312, 1.000000000000000000, 0.9510565162951535312, 1.000000000000000000, 0.9510565162951535312, 1.000000000000000000, 0.9510565162951535312, 1.000000000000000000, 0.9510565162951535312, 1.000000000000000000, 0.9510565162951535312, 1.000000000000000000, 0.9510565162951535312, 1.000000000000000000, 0.9510565162951535312, 1.000000000000000000, 0.9510565162951535312, 1.000000000000000000, 0.9510565162951535312, 1.000000000000000000, 0.9510565162951535312, 1.000000000000000000, 0.9510565162951535312, 1.000000000000000000, 0.9510565162951535312, 1.000000000000000000, 0.9510565162951535312, 1.000000000000000000, 0.9510565162951535312, 1.000000000000000000, 0.9510565162951535312, 1.000000000000000000, 0.9510565162951535312, 1.000000000000000000, 0.9510565162951535312, 1.000000000000000000, 0.9510565162951535312, 1.000000000000000000, 0.9510565162951535312, 1.000000000000000000, 0.9510565162951535312, 1.000000000000000000, 0.9510565162951535312, 1.000000000000000000, 0.9510565162951535312, 1.000000000000000000, 0.9510565162951535312, 1.000000000000000000, 0.9510565162951535312, 1.000000000000000000, 0.9510565162951535312, 1.000000000000000000, 0.9510565162951535312, 1.000000000000000000, 0.9510565162951535312, 1.000000000000000000, 0.9510565162951535312, 1.000000000000000000, 0.9510565162951535312, 1.000000000000000000, 0.9510565162951535312, 1.000000000000000000, 0.9510565162951535312, 1.000000000000000000, 0.9510565162951535312, 1.000000000000000000, 0.9510565162951535312, 1.000000000000000000, 0.9510565162951535312, 1.000000000000000000, 0.9510565162951535312, 1.000000000000000000, 0.9510565162951535312, 1.000000000000000000, 0.9510565162951535312, 1.000000000000000000, 0.9510565162951535312, 1.000000000000000000, 0.9510565162951535312, 1.000000000000000000, 0.9510565162951535312, 1.000000000000000000, 0.9510565162951535312, 1.000000000000000000, 0.9510565162951535312, 1.000000000000000000, 0.9510565162951535312, 1.000000000000000000, 0.9510565162951535312, 1.000000000000000000, 0.9510565162951535312, 1.000000000000000000, 0.9510565162951535312, 1.000000000000000000, 0.9510565162951535312, 1.000000000000000000, 0.9510565162951535312, 1.000000000000000000, 0.9510565162951535312, 1.000000000000000000, 0.9510565162951535312, 1.000000000000000000, 0.9510565162951535312, 1.000000000000000000, 0.9510565162951535312, 1.000000000000000000, 0.9510565162951535312, 1.000000000000000000, 0.9510565162951535312, 1.000000000000000000, 0.9510565162951535312, 1.000000000000000000, 0.9510565162951535312, 1.000000000000000000, 0.9510565162951535312, 1.000000000000000000, 0.9510565162951535312, 1.000000000000000000, 0.9510565162951535312, 1.000000000000000000, 0.9510565162951535312, 1.000000000000000000, 0.9510565162951535312, 1.000000000000000000, 0.9510565162951535312, 1.000000000000000000, 0.9510565162951535312, 1.000000000000000000, 0.9510565162951535312, 1.000000000000000000, 0.9510565162951535312, 1.000000000000000000, 0.9510565162951535312, 1.000000000000000000, 0.9510565162951535312, 1.000000000000000000, 0.9510565162951535312, 1.000000000000000000, 0.9510565162951535312, 1.000000000000000000, 0.9510565162951535312, 1.000000000000000000, 0.9510565162951535312, 1.000000000000000000, 0.9510565162951535312, 1.000000000000000000, 0.9510565162951535312, 1.000000000000000000, 0.9510565162951535312, 1.000000000000000000, 0.9510565162951535312, 1.000000000000000000, 0.9510565162951535312, 1.000000000000000000, 0.9510565162951535312, 1.000000000000000000, 0.9510565162951535312, 1.000000000000000000, 0.9510565162951535312, 1.000000000000000000, 0.9510565162951535312, 1.000000000000000000, 0.9510565162951535312, 1.000000000000000000, 0.9510565162951535312, 1.000000000000000000, 0.9510565162951535312, 1.000000000000000000, 0.9510565162951535312, 1.000000000000000000, 0.9510565162951535312, 1.000000000000000000, 0.9510565162951535312, 1.000000000000000000, 0.9510565162951535312, 1.000000000000000000, 0.9510565162951535312, 1.000000000000000000, 0.9510565162951535312, 1.000000000000000000, 0.9510565162951535312, 1.000000000000000000, 0.9510565162951535312, 1.000000000000000000, 0.9510565162951535312, 1.000000000000000000, 0.9674309245812854341, 0.9782075447827165426),
 ( 1.000000000000000000, 0.9510565162951535312, 1.000000000000000000, 0.9510565162951535312, 1.000000000000000000, 0.9510565162951535312, 1.000000000000000000, 0.9510565162951535312, 1.000000000000000000, 0.9510565162951535312, 1.000000000000000000, 0.9510565162951535312, 1.000000000000000000, 0.9510565162951535312, 1.000000000000000000, 0.9510565162951535312, 1.000000000000000000, 0.9510565162951535312, 1.000000000000000000, 0.9510565162951535312, 1.000000000000000000, 0.9510565162951535312, 1.000000000000000000, 0.9510565162951535312, 1.000000000000000000, 0.9510565162951535312, 1.000000000000000000, 0.9510565162951535312, 1.000000000000000000, 0.9510565162951535312, 1.000000000000000000, 0.9510565162951535312, 1.000000000000000000, 0.9510565162951535312, 1.000000000000000000, 0.9510565162951535312, 1.000000000000000000, 0.9510565162951535312, 1.000000000000000000, 0.9510565162951535312, 1.000000000000000000, 0.9510565162951535312, 1.000000000000000000, 0.9510565162951535312, 1.000000000000000000, 0.9510565162951535312, 1.000000000000000000, 0.9510565162951535312, 1.000000000000000000, 0.9510565162951535312, 1.000000000000000000, 0.9510565162951535312, 1.000000000000000000, 0.9510565162951535312, 1.000000000000000000, 0.9510565162951535312, 1.000000000000000000, 0.9510565162951535312, 1.000000000000000000, 0.9510565162951535312, 1.000000000000000000, 0.9510565162951535312, 1.000000000000000000, 0.9510565162951535312, 1.000000000000000000, 0.9510565162951535312, 1.000000000000000000, 0.9510565162951535312, 1.000000000000000000, 0.9510565162951535312, 1.000000000000000000, 0.9510565162951535312, 1.000000000000000000, 0.9510565162951535312, 1.000000000000000000, 0.9510565162951535312, 1.000000000000000000, 0.9510565162951535312, 1.000000000000000000, 0.9510565162951535312, 1.000000000000000000, 0.9510565162951535312, 1.000000000000000000, 0.9510565162951535312, 1.000000000000000000, 0.9510565162951535312, 1.000000000000000000, 0.9510565162951535312, 1.000000000000000000, 0.9510565162951535312, 1.000000000000000000, 0.9510565162951535312, 1.000000000000000000, 0.9510565162951535312, 1.000000000000000000, 0.9510565162951535312, 1.000000000000000000, 0.9510565162951535312, 1.000000000000000000, 0.9510565162951535312, 1.000000000000000000, 0.9510565162951535312, 1.000000000000000000, 0.9510565162951535312, 1.000000000000000000, 0.9510565162951535312, 1.000000000000000000, 0.9510565162951535312, 1.000000000000000000, 0.9510565162951535312, 1.000000000000000000, 0.9510565162951535312, 1.000000000000000000, 0.9510565162951535312, 1.000000000000000000, 0.9510565162951535312, 1.000000000000000000, 0.9510565162951535312, 1.000000000000000000, 0.9510565162951535312, 1.000000000000000000, 0.9510565162951535312, 1.000000000000000000, 0.9510565162951535312, 1.000000000000000000, 0.9510565162951535312, 1.000000000000000000, 0.9510565162951535312, 1.000000000000000000, 0.9510565162951535312, 1.000000000000000000, 0.9510565162951535312, 1.000000000000000000, 0.9510565162951535312, 1.000000000000000000, 0.9510565162951535312, 1.000000000000000000, 0.9510565162951535312, 1.000000000000000000, 0.9510565162951535312, 1.000000000000000000, 0.9510565162951535312, 1.000000000000000000, 0.9510565162951535312, 1.000000000000000000, 0.9510565162951535312, 1.000000000000000000, 0.9510565162951535312, 1.000000000000000000, 0.9510565162951535312, 1.000000000000000000, 0.9510565162951535312, 1.000000000000000000, 0.9510565162951535312, 1.000000000000000000, 0.9510565162951535312, 1.000000000000000000, 0.9510565162951535312, 1.000000000000000000, 0.9510565162951535312, 1.000000000000000000, 0.9510565162951535312, 1.000000000000000000, 0.9510565162951535312, 1.000000000000000000, 0.9510565162951535312, 1.000000000000000000, 0.9510565162951535312, 1.000000000000000000, 0.9510565162951535312, 1.000000000000000000, 0.9510565162951535312, 1.000000000000000000, 0.9510565162951535312, 1.000000000000000000, 0.9510565162951535312, 1.000000000000000000, 0.9510565162951535312, 1.000000000000000000, 0.9510565162951535312, 1.000000000000000000, 0.9510565162951535312, 1.000000000000000000, 0.9510565162951535312, 1.000000000000000000, 0.9510565162951535312, 1.000000000000000000, 0.9510565162951535312, 1.000000000000000000, 0.9510565162951535312, 1.000000000000000000, 0.9510565162951535312, 1.000000000000000000, 0.9510565162951535312, 1.000000000000000000, 0.9510565162951535312, 1.000000000000000000, 0.9510565162951535312, 1.000000000000000000, 0.9510565162951535312, 1.000000000000000000, 0.9510565162951535312, 1.000000000000000000, 0.9510565162951535312, 1.000000000000000000, 0.9510565162951535312, 1.000000000000000000, 0.9510565162951535312, 1.000000000000000000, 0.9510565162951535312, 1.000000000000000000, 0.9510565162951535312, 1.000000000000000000, 0.9510565162951535312, 1.000000000000000000, 0.9510565162951535312, 1.000000000000000000, 0.9510565162951535312, 1.000000000000000000, 0.9510565162951535312, 1.000000000000000000, 0.9510565162951535312, 1.000000000000000000, 0.9510565162951535312, 1.000000000000000000, 0.9510565162951535312, 1.000000000000000000, 0.9510565162951535312, 1.000000000000000000, 0.9510565162951535312, 1.000000000000000000, 0.9510565162951535312, 1.000000000000000000, 0.9510565162951535312, 1.000000000000000000, 0.9510565162951535312, 1.000000000000000000, 0.9510565162951535312, 1.000000000000000000, 0.9510565162951535312, 1.000000000000000000, 0.9510565162951535312, 1.000000000000000000, 0.9510565162951535312, 1.000000000000000000, 0.9510565162951535312, 1.000000000000000000, 0.9510565162951535312, 1.000000000000000000, 0.9510565162951535312, 1.000000000000000000, 0.9510565162951535312, 1.000000000000000000, 0.9510565162951535312, 1.000000000000000000, 0.9510565162951535312, 1.000000000000000000, 0.9510565162951535312, 1.000000000000000000, 0.9510565162951535312, 1.000000000000000000, 0.9510565162951535312, 1.000000000000000000, 0.9510565162951535312, 1.000000000000000000, 0.9510565162951535312, 1.000000000000000000, 0.9510565162951535312, 1.000000000000000000, 0.9510565162951535312, 1.000000000000000000, 0.9510565162951535312, 1.000000000000000000, 0.9510565162951535312, 1.000000000000000000, 0.9510565162951535312, 1.000000000000000000, 0.9510565162951535312, 1.000000000000000000, 0.9510565162951535312, 1.000000000000000000, 0.9510565162951535312, 1.000000000000000000, 0.9510565162951535312, 1.000000000000000000, 0.9510565162951535312, 1.000000000000000000, 0.9510565162951535312, 1.000000000000000000, 0.9510565162951535312, 1.000000000000000000, 0.9510565162951535312, 1.000000000000000000, 0.9510565162951535312, 1.000000000000000000, 0.9510565162951535312, 1.000000000000000000, 0.9510565162951535312, 1.000000000000000000, 0.9510565162951535312, 1.000000000000000000, 0.9510565162951535312, 1.000000000000000000, 0.9510565162951535312, 1.000000000000000000, 0.9510565162951535312, 1.000000000000000000, 0.9510565162951535312, 1.000000000000000000, 0.9510565162951535312, 1.000000000000000000, 0.9510565162951535312, 1.000000000000000000, 0.9510565162951535312, 1.000000000000000000, 0.9510565162951535312, 1.000000000000000000, 0.9510565162951535312, 1.000000000000000000, 0.9510565162951535312, 1.000000000000000000, 0.9510565162951535312, 1.000000000000000000, 0.9510565162951535312, 1.000000000000000000, 0.9510565162951535312, 1.000000000000000000, 0.9510565162951535312, 1.000000000000000000, 0.9510565162951535312, 1.000000000000000000, 0.9510565162951535312, 1.000000000000000000, 0.9510565162951535312, 1.000000000000000000, 0.9510565162951535312, 1.000000000000000000, 0.9510565162951535312, 1.000000000000000000, 0.9510565162951535312, 1.000000000000000000, 0.9510565162951535312, 1.000000000000000000, 0.9510565162951535312, 1.000000000000000000, 0.9510565162951535312, 1.000000000000000000, 0.9510565162951535312, 1.000000000000000000, 0.9510565162951535312, 1.000000000000000000, 0.9510565162951535312, 1.000000000000000000, 0.9674309245812854341, 0.9782075447827165426) ) ) 
 REPRESENTATION_ITEM ( '' )  SURFACE ( )  );
#7487 = CARTESIAN_POINT ( 'NONE',  ( 11.62722211559520424, 54.17461734033530973, 6.859929859063566226 ) ) ;
#7488 = VERTEX_POINT ( 'NONE', #12320 ) ;
#7489 = DIRECTION ( 'NONE',  ( -8.862145109134287319E-17, 1.000000000000000000, 0.000000000000000000 ) ) ;
#7490 = ORIENTED_EDGE ( 'NONE', *, *, #9438, .T. ) ;
#7491 = CARTESIAN_POINT ( 'NONE',  ( 6.758386942186555224, 66.93077324841343057, -11.70470293470154921 ) ) ;
#7492 = CARTESIAN_POINT ( 'NONE',  ( 11.37499999999960210, -22.85937499999996092, 4.711679271994916540 ) ) ;
#7493 = EDGE_CURVE ( 'NONE', #8734, #6926, #9425, .T. ) ;
#7494 = FACE_OUTER_BOUND ( 'NONE', #15199, .T. ) ;
#7495 = DIRECTION ( 'NONE',  ( 0.000000000000000000, 0.000000000000000000, 1.000000000000000000 ) ) ;
#7496 = DIRECTION ( 'NONE',  ( 0.000000000000000000, 0.000000000000000000, -1.000000000000000000 ) ) ;
#7497 = CARTESIAN_POINT ( 'NONE',  ( -10.92172942406178926, 5.629999999999996341, -7.935100905948389460 ) ) ;
#7498 = CARTESIAN_POINT ( 'NONE',  ( 11.59770818944004134, 72.17250917721062820, 6.911720118166459592 ) ) ;
#7499 = CARTESIAN_POINT ( 'NONE',  ( 9.520470885617717371, 32.73000000000001108, -6.917026985038131848 ) ) ;
#7500 = CARTESIAN_POINT ( 'NONE',  ( -4.171729424061787483, 52.32999999999999829, -12.83926296998457417 ) ) ;
#7501 = CARTESIAN_POINT ( 'NONE',  ( -5.864567678274497986, 52.39362192653054962, -12.15966658976413584 ) ) ;
#7502 = CARTESIAN_POINT ( 'NONE',  ( 2.607531440858944223E-15, 51.18000000000000682, -14.19474002721660355 ) ) ;
#7503 = CARTESIAN_POINT ( 'NONE',  ( 18.99999999999999289, 7.773118517290098062, 1.732050807568941586 ) ) ;
#7504 = CARTESIAN_POINT ( 'NONE',  ( -11.34163888740973825, 68.20410188839301213, 7.325683172086050909 ) ) ;
#7505 = CARTESIAN_POINT ( 'NONE',  ( 7.714727599200458030, -53.07187499999987068, -18.62499999999934985 ) ) ;
#7506 = LINE ( 'NONE', #7332, #3936 ) ;
#7507 = CARTESIAN_POINT ( 'NONE',  ( 13.16986379960055054, -52.03124999999987921, -13.16986379959834430 ) ) ;
#7508 = CARTESIAN_POINT ( 'NONE',  ( -8.342243388378552282, 65.36176465702267535, 10.61802124403202541 ) ) ;
#7509 = CARTESIAN_POINT ( 'NONE',  ( 10.17549044795671165, 7.957350711246245822, -15.32050807568889539 ) ) ;
#7510 = CARTESIAN_POINT ( 'NONE',  ( 8.197819711906403128, 7.962112819640459804, -16.44350439286869303 ) ) ;
#7511 = CARTESIAN_POINT ( 'NONE',  ( 13.50000000000000000, 25.43000000000000682, 1.734723475976807094E-15 ) ) ;
#7512 = EDGE_CURVE ( 'NONE', #15397, #10663, #5001, .T. ) ;
#7513 = ORIENTED_EDGE ( 'NONE', *, *, #6025, .F. ) ;
#7514 = CARTESIAN_POINT ( 'NONE',  ( -11.76794919243112325, 33.07999999999999119, 3.823638476888994830 ) ) ;
#7515 = VECTOR ( 'NONE', #14662, 1000.000000000000000 ) ;
#7516 = CARTESIAN_POINT ( 'NONE',  ( -2.869462971216817593, 40.28317531134132423, -13.19152261891324684 ) ) ;
#7517 = CARTESIAN_POINT ( 'NONE',  ( -12.91569140150223483, 31.78915324831410771, -3.928925989131344387 ) ) ;
#7518 = CARTESIAN_POINT ( 'NONE',  ( 3.660164850489102228, 74.81160598410180285, 12.99436167334853387 ) ) ;
#7519 = CARTESIAN_POINT ( 'NONE',  ( 10.91662889535533232, 1.083605698617470082E-14, -3.544256338779125937 ) ) ;
#7520 = CARTESIAN_POINT ( 'NONE',  ( 690.7486963872878505, 879.4553902717701703, 1297.674793841596738 ) ) ;
#7521 = CARTESIAN_POINT ( 'NONE',  ( 13.50000000000000355, 77.58000000000001251, -4.386415899144233244 ) ) ;
#7522 = CARTESIAN_POINT ( 'NONE',  ( 13.09516998140269806, 51.54708633261468265, -3.291187128613837665 ) ) ;
#7523 = VECTOR ( 'NONE', #17165, 1000.000000000000000 ) ;
#7524 = CARTESIAN_POINT ( 'NONE',  ( -13.34762704780204601, 38.00086476210552888, 2.022771026582171672 ) ) ;
#7525 = CARTESIAN_POINT ( 'NONE',  ( 11.32356926193947722, 36.70559104637850822, -7.350409248560260345 ) ) ;
#7526 = CARTESIAN_POINT ( 'NONE',  ( -8.043339635997652337, -67.60624999999984652, 8.043339635996300530 ) ) ;
#7527 = CARTESIAN_POINT ( 'NONE',  ( 19.00000000000000711, 7.773118517290098062, -1.732050807568807249 ) ) ;
#7528 = CARTESIAN_POINT ( 'NONE',  ( -3.390861109279693419, 77.55806408242118266, 13.06768226514972397 ) ) ;
#7529 = CARTESIAN_POINT ( 'NONE',  ( 2.894739590358088936E-06, 0.6800804143413337055, 13.49999999999938360 ) ) ;
#7530 = CARTESIAN_POINT ( 'NONE',  ( 8.270203509715585710, 41.99506318914406222, 10.67024559312394949 ) ) ;
#7531 = CARTESIAN_POINT ( 'NONE',  ( 13.48921303027230323, 48.41115837036991110, 0.5474105875851942304 ) ) ;
#7532 = CARTESIAN_POINT ( 'NONE',  ( -9.520470885617717371, 13.23000000000001997, 6.917026985038133624 ) ) ;
#7533 = EDGE_LOOP ( 'NONE', ( #16126, #4653 ) ) ;
#7534 = CARTESIAN_POINT ( 'NONE',  ( 2.272985001014427393E-15, 62.17999999999999972, -12.37355403259654807 ) ) ;
#7535 = CARTESIAN_POINT ( 'NONE',  ( -4.711679271994916540, -20.84687499999993321, 11.37499999999960565 ) ) ;
#7536 = DIRECTION ( 'NONE',  ( 0.000000000000000000, 0.000000000000000000, -1.000000000000000000 ) ) ;
#7537 = ADVANCED_FACE ( 'NONE', ( #8008 ), #9007, .T. ) ;
#7538 = CARTESIAN_POINT ( 'NONE',  ( 11.76794919243112680, 29.58000000000000540, -3.823638476888993942 ) ) ;
#7539 = CARTESIAN_POINT ( 'NONE',  ( -4.886222543804722207, 80.92999999999999261, -11.77926528190734423 ) ) ;
#7540 = CARTESIAN_POINT ( 'NONE',  ( -7.576616670048093940E-16, 33.67999999999999972, 12.37355403259654985 ) ) ;
#7541 = VECTOR ( 'NONE', #1977, 1000.000000000000000 ) ;
#7542 = CARTESIAN_POINT ( 'NONE',  ( -13.16986379960055231, -43.70624999999989768, 13.16986379959834252 ) ) ;
#7543 = CARTESIAN_POINT ( 'NONE',  ( 10.92172942406178926, 78.13000000000000966, 7.935100905948387684 ) ) ;
#7544 = CARTESIAN_POINT ( 'NONE',  ( -9.520470885617717371, 45.22999999999999687, 6.917026985038133624 ) ) ;
#7545 = CARTESIAN_POINT ( 'NONE',  ( -9.957257356812577953, 59.28301542262214952, 9.116086396973207329 ) ) ;
#7546 = CARTESIAN_POINT ( 'NONE',  ( 12.67739711398077596, 45.26084057892622070, 4.680113183824990308 ) ) ;
#7547 = PLANE ( 'NONE',  #350 ) ;
#7548 = CARTESIAN_POINT ( 'NONE',  ( 3.904524039968586990, 80.82037356980362119, 12.92421824227555760 ) ) ;
#7549 = CARTESIAN_POINT ( 'NONE',  ( 13.49560925073025430, 30.44260291568510013, -0.3671350940585685896 ) ) ;
#7550 = CARTESIAN_POINT ( 'NONE',  ( -13.45459026473954545, 55.96837007948868603, 1.107234817202036092 ) ) ;
#7551 = LINE ( 'NONE', #14240, #185 ) ;
#7552 = CARTESIAN_POINT ( 'NONE',  ( 9.123705676088246008, 63.82520120319571078, -9.962466972052720138 ) ) ;
#7553 = CARTESIAN_POINT ( 'NONE',  ( 24.73863375370599016, 5.918584287042170544, -7.999999999999936051 ) ) ;
#7554 = CARTESIAN_POINT ( 'NONE',  ( 11.95191421947951227, 39.66185529926528375, -6.277088439489496352 ) ) ;
#7555 = EDGE_LOOP ( 'NONE', ( #15896, #1535, #15760, #63 ) ) ;
#7556 = CARTESIAN_POINT ( 'NONE',  ( -7.444042646070399449, 61.45851055580283173, -11.26259205123165863 ) ) ;
#7557 = ORIENTED_EDGE ( 'NONE', *, *, #16322, .F. ) ;
#7558 = EDGE_CURVE ( 'NONE', #149, #2392, #16369, .T. ) ;
#7559 = VERTEX_POINT ( 'NONE', #16101 ) ;
#7560 = CARTESIAN_POINT ( 'NONE',  ( 8.343458848123578520, 32.97999999999999687, 11.48378591275254124 ) ) ;
#7561 = CARTESIAN_POINT ( 'NONE',  ( 1.561832610794586538E-12, -37.46249999999991331, -18.62500000000000000 ) ) ;
#7562 = CARTESIAN_POINT ( 'NONE',  ( 10.48475946639971923, 48.10524804026067613, 8.504759123327721326 ) ) ;
#7563 = B_SPLINE_CURVE_WITH_KNOTS ( 'NONE', 3,
 ( #12685, #5722, #9615, #6958, #8376, #401, #1800, #14966, #8289, #1540, #12517, #16651, #229, #13732, #5634, #575, #10928, #16296 ),
 .UNSPECIFIED., .F., .F.,
 ( 4, 2, 2, 2, 2, 2, 2, 2, 4 ),
 ( 2.030049010680397961E-07, 0.0005272941439305969162, 0.001054385282960125948, 0.001581476421989654870, 0.002108567561019183793, 0.002635658700048712499, 0.003162749839078241639, 0.003689840978107770779, 0.004216932117137299485 ),
 .UNSPECIFIED. ) ;
#7564 = CARTESIAN_POINT ( 'NONE',  ( 2.430993506533023485, 58.09259044382305603, -13.27931747540271701 ) ) ;
#7565 = CARTESIAN_POINT ( 'NONE',  ( 11.05296802401333700, 78.72228217906655345, -7.752379973867670415 ) ) ;
#7566 = CARTESIAN_POINT ( 'NONE',  ( 11.76794919243112680, 76.57999999999998408, -3.823638476888993942 ) ) ;
#7567 = CARTESIAN_POINT ( 'NONE',  ( -8.691771469529815392E-16, 40.67999999999999972, 14.19474002721660355 ) ) ;
#7568 = CARTESIAN_POINT ( 'NONE',  ( 8.858858224111887836, 3.937340487231678143E-15, -8.306292331654377747 ) ) ;
#7569 = CARTESIAN_POINT ( 'NONE',  ( 13.50000000000000000, 1.430000000000014593, 1.734723475976807094E-15 ) ) ;
#7570 = CARTESIAN_POINT ( 'NONE',  ( 10.59289456970070553, -99.99999999999994316, 4.700358225852117933 ) ) ;
#7571 = DIRECTION ( 'NONE',  ( 0.000000000000000000, -1.000000000000000000, 0.000000000000000000 ) ) ;
#7572 = CARTESIAN_POINT ( 'NONE',  ( -11.37499999999960743, -16.68437499999993889, -4.711679271994912099 ) ) ;
#7573 = CARTESIAN_POINT ( 'NONE',  ( -13.49999999999999822, 78.78000000000000114, -4.386415899144240349 ) ) ;
#7574 = CARTESIAN_POINT ( 'NONE',  ( 3.084857733306134442, 34.06908001793591723, -13.14282405559487721 ) ) ;
#7575 = VERTEX_POINT ( 'NONE', #4011 ) ;
#7576 = CARTESIAN_POINT ( 'NONE',  ( 8.376189165296050732, 10.00005005279484038, 10.58723084571193596 ) ) ;
#7577 = ORIENTED_EDGE ( 'NONE', *, *, #11541, .T. ) ;
#7578 = CARTESIAN_POINT ( 'NONE',  ( 17.14738331135994187, 7.815232041205462998, -7.999999999999963585 ) ) ;
#7579 = CARTESIAN_POINT ( 'NONE',  ( -8.043339635997654113, -93.65624999999977263, 8.043339635996302306 ) ) ;
#7580 = DIRECTION ( 'NONE',  ( 0.000000000000000000, 1.000000000000000000, 0.000000000000000000 ) ) ;
#7581 = CYLINDRICAL_SURFACE ( 'NONE', #14058, 1.999999999999998224 ) ;
#7582 = FACE_OUTER_BOUND ( 'NONE', #8805, .T. ) ;
#7583 = CARTESIAN_POINT ( 'NONE',  ( 2.445080149700053643E-15, 39.17999999999999972, -13.50000000000000000 ) ) ;
#7584 = CARTESIAN_POINT ( 'NONE',  ( 2.479997878773285702, 71.76914845574894741, 13.27026003324255932 ) ) ;
#7585 = CARTESIAN_POINT ( 'NONE',  ( 8.343458848123578520, 50.97999999999999687, 11.48378591275254124 ) ) ;
#7586 = CARTESIAN_POINT ( 'NONE',  ( -0.3693890974730637544, 71.66671813216132136, 13.49494611521610388 ) ) ;
#7587 = CARTESIAN_POINT ( 'NONE',  ( 7.500000000000000888, -18.00000000000000355, -9.000000000000001776 ) ) ;
#7588 = CARTESIAN_POINT ( 'NONE',  ( 13.16986379959834075, -47.86874999999988489, 13.16986379960055231 ) ) ;
#7589 = EDGE_CURVE ( 'NONE', #5051, #14868, #14774, .T. ) ;
#7590 = CARTESIAN_POINT ( 'NONE',  ( -4.236652733600446474, 68.52767330046546590, 12.81802689691797248 ) ) ;
#7591 = CARTESIAN_POINT ( 'NONE',  ( 13.16986379959834075, -64.51874999999984084, 13.16986379960055231 ) ) ;
#7592 = CARTESIAN_POINT ( 'NONE',  ( 5.205044219673900407, 54.99195532384126750, -12.45725450968071435 ) ) ;
#7593 = AXIS2_PLACEMENT_3D ( 'NONE', #16461, #1525, #8272 ) ;
#7594 = CARTESIAN_POINT ( 'NONE',  ( 13.16986379959834075, -14.56874999999996589, 13.16986379960055231 ) ) ;
#7595 = CARTESIAN_POINT ( 'NONE',  ( -4.275606992132293449, 65.52616433460548251, 12.83507194185807343 ) ) ;
#7596 = CYLINDRICAL_SURFACE ( 'NONE', #3660, 13.50000000000000000 ) ;
#7597 = CARTESIAN_POINT ( 'NONE',  ( -10.81341862071700888, 35.23731261369557899, 8.112425484178327650 ) ) ;
#7598 = CARTESIAN_POINT ( 'NONE',  ( -13.49999999999999822, 23.77999999999999403, -4.386415899144240349 ) ) ;
#7599 = ORIENTED_EDGE ( 'NONE', *, *, #1923, .F. ) ;
#7600 = CARTESIAN_POINT ( 'NONE',  ( -8.343458848123582072, 9.379999999999999005, 11.48378591275253768 ) ) ;
#7601 = CARTESIAN_POINT ( 'NONE',  ( 0.000000000000000000, 5.918584287042170544, 0.000000000000000000 ) ) ;
#7602 = CARTESIAN_POINT ( 'NONE',  ( -13.34330937586820198, 32.00188493264690948, 2.051126618964131065 ) ) ;
#7603 = CARTESIAN_POINT ( 'NONE',  ( 7.833167725097554879, 74.97547919491985624, 10.99603809193803805 ) ) ;
#7604 = CARTESIAN_POINT ( 'NONE',  ( 13.49758425966062170, 60.40291432109311387, 0.7880808366232104900 ) ) ;
#7605 = CARTESIAN_POINT ( 'NONE',  ( -8.549982208541774191E-16, 0.6799999999999988276, 14.19474002721660355 ) ) ;
#7606 = CARTESIAN_POINT ( 'NONE',  ( 13.50000000000000000, 62.42999999999999972, 1.653273178848926867E-15 ) ) ;
#7607 = B_SPLINE_CURVE_WITH_KNOTS ( 'NONE', 3,
 ( #16809, #644, #16552, #7286 ),
 .UNSPECIFIED., .F., .F.,
 ( 4, 4 ),
 ( 2.376698214937377243E-07, 0.007646667280170312518 ),
 .UNSPECIFIED. ) ;
#7608 = AXIS2_PLACEMENT_3D ( 'NONE', #1240, #6653, #16162 ) ;
#7609 =( NAMED_UNIT ( * ) PLANE_ANGLE_UNIT ( ) SI_UNIT ( $, .RADIAN. ) );
#7610 = CARTESIAN_POINT ( 'NONE',  ( 10.92172942406178926, 74.12999999999999545, 7.935100905948387684 ) ) ;
#7611 = CARTESIAN_POINT ( 'NONE',  ( 13.47580859582107671, 51.45868852590849940, -0.8310248978193689462 ) ) ;
#7612 = CARTESIAN_POINT ( 'NONE',  ( -12.66827453022257721, 38.09892961922952281, 4.669650815327920590 ) ) ;
#7613 = CARTESIAN_POINT ( 'NONE',  ( 11.60544498200051322, 36.68704456685242121, -6.899790396877484078 ) ) ;
#7614 = CARTESIAN_POINT ( 'NONE',  ( 11.37500000000039613, -58.24062499999988063, -4.711679271993002516 ) ) ;
#7615 = CARTESIAN_POINT ( 'NONE',  ( 9.708203932499371192, 2.596025403784447683, -7.053423027509677645 ) ) ;
#7616 = CARTESIAN_POINT ( 'NONE',  ( -3.875797842856171904, 77.54063790311734294, 12.93175633931209134 ) ) ;
#7617 = CARTESIAN_POINT ( 'NONE',  ( -2.094509993892973210, 80.60457276769930957, 13.33968883972704944 ) ) ;
#7618 = CARTESIAN_POINT ( 'NONE',  ( 5.374832067266447133, 41.87461798944549685, 12.38404490627867105 ) ) ;
#7619 = ORIENTED_EDGE ( 'NONE', *, *, #6216, .T. ) ;
#7620 = CIRCLE ( 'NONE', #1106, 12.00000000000000178 ) ;
#7621 = CARTESIAN_POINT ( 'NONE',  ( -9.520470885617717371, 10.23000000000000220, 6.917026985038133624 ) ) ;
#7622 = ORIENTED_EDGE ( 'NONE', *, *, #721, .F. ) ;
#7623 = CARTESIAN_POINT ( 'NONE',  ( 11.76794919243112325, 58.42999999999999261, 1.441158131103945434E-15 ) ) ;
#7624 = CARTESIAN_POINT ( 'NONE',  ( -9.552639591052204498E-13, -88.48749999999975557, 11.37500000000000178 ) ) ;
#7625 = CARTESIAN_POINT ( 'NONE',  ( 2.138189944381238661, 55.75688142232026934, 13.50000000000000000 ) ) ;
#7626 = CARTESIAN_POINT ( 'NONE',  ( 1.921271214528800453, 76.11093797914737991, -13.37211609379623667 ) ) ;
#7627 = CARTESIAN_POINT ( 'NONE',  ( 13.16986379960055054, -68.68124999999983515, -13.16986379959834430 ) ) ;
#7628 = CARTESIAN_POINT ( 'NONE',  ( 1.293886105031521572, 65.72652579852442045, 13.44153297767990018 ) ) ;
#7629 = DIRECTION ( 'NONE',  ( 0.5000000000000013323, 0.000000000000000000, -0.8660254037844379305 ) ) ;
#7630 = CARTESIAN_POINT ( 'NONE',  ( 11.76794919243112325, 52.28000000000000114, 3.823638476888996607 ) ) ;
#7631 = CARTESIAN_POINT ( 'NONE',  ( -7.416407864998772581, 9.613974596215609125, -10.20780970022453360 ) ) ;
#7632 = CARTESIAN_POINT ( 'NONE',  ( -11.07257681465629773, 59.22107823441397301, 7.723217015962382526 ) ) ;
#7633 = EDGE_CURVE ( 'NONE', #6360, #3099, #8182, .T. ) ;
#7634 = CARTESIAN_POINT ( 'NONE',  ( 10.59059375150318516, 45.11097004264419752, 8.373194485267964282 ) ) ;
#7635 = CARTESIAN_POINT ( 'NONE',  ( 11.15661179884298981, 69.71598163396143377, -7.601483556432171440 ) ) ;
#7636 = EDGE_CURVE ( 'NONE', #13489, #13982, #539, .T. ) ;
#7637 = CARTESIAN_POINT ( 'NONE',  ( 3.040576530018048729, 80.78928174342134128, 13.16481631334213098 ) ) ;
#7638 = CARTESIAN_POINT ( 'NONE',  ( 13.28204714884621396, 30.34495749442142198, 2.416062439415011642 ) ) ;
#7639 = CARTESIAN_POINT ( 'NONE',  ( -13.24809406675781176, 55.83842994404133719, -2.595915310630025452 ) ) ;
#7640 = CARTESIAN_POINT ( 'NONE',  ( -12.82172618473797776, 50.08243652013945280, 4.237200570767894803 ) ) ;
#7641 = CARTESIAN_POINT ( 'NONE',  ( 2.757549515546722230, 64.08084869351907287, -13.21536860246509271 ) ) ;
#7642 = DIRECTION ( 'NONE',  ( 0.000000000000000000, 1.000000000000000000, 0.000000000000000000 ) ) ;
#7643 = CARTESIAN_POINT ( 'NONE',  ( 10.33236877401481735, 39.76306948997951451, -8.688624863794741415 ) ) ;
#7644 = ORIENTED_EDGE ( 'NONE', *, *, #15559, .F. ) ;
#7645 = CARTESIAN_POINT ( 'NONE',  ( -10.07187023573678353, 61.58299827724115261, -8.989296097550834475 ) ) ;
#7646 = CARTESIAN_POINT ( 'NONE',  ( 3.636496289402157078, 6.030000000000007354, -11.19198476289190936 ) ) ;
#7647 = VERTEX_POINT ( 'NONE', #1346 ) ;
#7648 = AXIS2_PLACEMENT_3D ( 'NONE', #3440, #8855, #16697 ) ;
#7649 = CARTESIAN_POINT ( 'NONE',  ( -8.694191427202177636, 40.51460945123136526, -10.32880532873150869 ) ) ;
#7650 = ORIENTED_EDGE ( 'NONE', *, *, #5216, .T. ) ;
#7651 = CARTESIAN_POINT ( 'NONE',  ( 10.92172942406179104, 33.73000000000001108, -7.935100905948385908 ) ) ;
#7652 = CARTESIAN_POINT ( 'NONE',  ( -1.564113515457998572E-12, -29.13749999999993179, 18.62500000000000000 ) ) ;
#7653 = CARTESIAN_POINT ( 'NONE',  ( 3.279879460145345593, 47.79795238127255885, 13.09551564182569017 ) ) ;
#7654 = CARTESIAN_POINT ( 'NONE',  ( 10.91216525745976895, 57.73057897943527905, -7.953499367341933635 ) ) ;
#7655 = CARTESIAN_POINT ( 'NONE',  ( 6.542932766149395896, 78.93933411452208304, -11.81244280098690780 ) ) ;
#7656 = CARTESIAN_POINT ( 'NONE',  ( -7.272992578804310604, 78.38000000000000966, 10.01041549318726709 ) ) ;
#7657 = FACE_OUTER_BOUND ( 'NONE', #16863, .T. ) ;
#7658 = DIRECTION ( 'NONE',  ( 0.000000000000000000, -1.000000000000000000, 0.000000000000000000 ) ) ;
#7659 = EDGE_CURVE ( 'NONE', #1796, #2326, #15192, .T. ) ;
#7660 =( GEOMETRIC_REPRESENTATION_CONTEXT ( 3 ) GLOBAL_UNCERTAINTY_ASSIGNED_CONTEXT ( ( #11405 ) ) GLOBAL_UNIT_ASSIGNED_CONTEXT ( ( #529, #14124, #16870 ) ) REPRESENTATION_CONTEXT ( 'NONE', 'WORKASPACE' ) );
#7661 = CARTESIAN_POINT ( 'NONE',  ( 18.62500000000000000, 0.000000000000000000, 1.560692158462880521E-12 ) ) ;
#7662 = CARTESIAN_POINT ( 'NONE',  ( 11.37500000000000178, -59.34999999999983800, 9.531744055041752924E-13 ) ) ;
#7663 = DIRECTION ( 'NONE',  ( 0.000000000000000000, -1.000000000000000000, 0.000000000000000000 ) ) ;
#7664 = CARTESIAN_POINT ( 'NONE',  ( 3.151976139588944736, 34.06667296235463027, -13.12692461614821582 ) ) ;
#7665 = ORIENTED_EDGE ( 'NONE', *, *, #237, .F. ) ;
#7666 = CARTESIAN_POINT ( 'NONE',  ( 15.58845726811984811, 0.000000000000000000, 11.00000000000007283 ) ) ;
#7667 = EDGE_LOOP ( 'NONE', ( #8347, #1962, #820, #1019 ) ) ;
#7668 = CARTESIAN_POINT ( 'NONE',  ( -11.37500000000039613, -16.61562499999998010, 4.711679271993000739 ) ) ;
#7669 = CARTESIAN_POINT ( 'NONE',  ( 4.961522565702499499, 77.85890369619608009, 12.55714296570731392 ) ) ;
#7670 = CARTESIAN_POINT ( 'NONE',  ( -7.187129287260045629, 59.41245409490487361, 11.42782594799617968 ) ) ;
#7671 = CARTESIAN_POINT ( 'NONE',  ( 15.32106749056511852, 7.956441901775577641, 10.18076046065000817 ) ) ;
#7672 = DIRECTION ( 'NONE',  ( 0.000000000000000000, -0.000000000000000000, 1.000000000000000000 ) ) ;
#7673 = CARTESIAN_POINT ( 'NONE',  ( 10.92172942406178926, 57.13000000000000256, 7.935100905948387684 ) ) ;
#7674 = CARTESIAN_POINT ( 'NONE',  ( -2.520299001384201265, 71.58939712408532330, 13.26745337539860259 ) ) ;
#7675 = EDGE_CURVE ( 'NONE', #5870, #9540, #2022, .T. ) ;
#7676 = FACE_OUTER_BOUND ( 'NONE', #15542, .T. ) ;
#7677 = CARTESIAN_POINT ( 'NONE',  ( 1.561832610794586740E-12, 3.087500000000011458, -18.62500000000000000 ) ) ;
#7678 = CARTESIAN_POINT ( 'NONE',  ( 1.939380092513621090, 68.74973318765675856, 13.35997747337515307 ) ) ;
#7679 = CARTESIAN_POINT ( 'NONE',  ( 13.16986379960055054, -35.38124999999991616, -13.16986379959834430 ) ) ;
#7680 = DIRECTION ( 'NONE',  ( 0.000000000000000000, 1.000000000000000000, 0.000000000000000000 ) ) ;
#7681 = CARTESIAN_POINT ( 'NONE',  ( 18.62499999999934630, -65.55937499999984652, 7.714727599200467800 ) ) ;
#7682 = CARTESIAN_POINT ( 'NONE',  ( -3.417358507291479164, 65.55712218665007640, 13.09022083234078870 ) ) ;
#7683 = CARTESIAN_POINT ( 'NONE',  ( -11.52888015854885317, 80.93000000000003524, -3.329402692648984363 ) ) ;
#7684 = CARTESIAN_POINT ( 'NONE',  ( -6.469357084119882195, 35.44227298974823270, 11.85135619912656502 ) ) ;
#7685 = CARTESIAN_POINT ( 'NONE',  ( -10.92172942406179104, 24.23000000000000043, 7.935100905948385908 ) ) ;
#7686 = ORIENTED_EDGE ( 'NONE', *, *, #1587, .F. ) ;
#7687 = CARTESIAN_POINT ( 'NONE',  ( 9.520470885617717371, 31.72999999999999332, -6.917026985038131848 ) ) ;
#7688 = CARTESIAN_POINT ( 'NONE',  ( -13.17209843300189576, 32.03655692023156831, 3.006699176096832460 ) ) ;
#7689 = CARTESIAN_POINT ( 'NONE',  ( -8.000000000000145661, 0.000000000000000000, 17.32050807568870709 ) ) ;
#7690 = CARTESIAN_POINT ( 'NONE',  ( 13.07535219888350753, 60.31039798475667624, 3.359492778058866591 ) ) ;
#7691 = CARTESIAN_POINT ( 'NONE',  ( 13.50000000000000355, -10.42000000000000703, -4.386415899144233244 ) ) ;
#7692 = CARTESIAN_POINT ( 'NONE',  ( -11.70956602232489630, 53.18020972713351568, 6.735112246977101869 ) ) ;
#7693 = AXIS2_PLACEMENT_3D ( 'NONE', #3104, #5700, #8531 ) ;
#7694 = CARTESIAN_POINT ( 'NONE',  ( 3.636496289402157078, 59.03000000000000114, -11.19198476289190936 ) ) ;
#7695 = ITEM_DEFINED_TRANSFORMATION ( 'NONE', 'NONE', #5109,  #16654 ) ;
#7696 = CARTESIAN_POINT ( 'NONE',  ( 13.49481123919801639, 51.44323841525638130, -0.3855105674034914887 ) ) ;
#7697 = CARTESIAN_POINT ( 'NONE',  ( -13.47601568130759198, 37.90221951456256733, -0.8043930999376557311 ) ) ;
#7698 = CARTESIAN_POINT ( 'NONE',  ( 13.22368575055132212, 36.52637389139642465, -2.727991382493684114 ) ) ;
#7699 = CARTESIAN_POINT ( 'NONE',  ( 11.37500000000039613, -41.59062499999991758, -4.711679271993002516 ) ) ;
#7700 = CARTESIAN_POINT ( 'NONE',  ( -2.197460307225001408, 74.60102142208326370, 13.32837458805170527 ) ) ;
#7701 = CARTESIAN_POINT ( 'NONE',  ( -10.58220227879168540, 77.24934925134837727, 8.383323893021028539 ) ) ;
#7702 = CIRCLE ( 'NONE', #8557, 2.000000000000001776 ) ;
#7703 = CARTESIAN_POINT ( 'NONE',  ( -5.506042237581730170, 80.48045121655667344, 12.33370346659203953 ) ) ;
#7704 = CARTESIAN_POINT ( 'NONE',  ( 7.500000000000001776, 108.6199039925687089, -2.572187159835566117 ) ) ;
#7705 = ORIENTED_EDGE ( 'NONE', *, *, #13536, .F. ) ;
#7706 = CARTESIAN_POINT ( 'NONE',  ( -7.272992578804310604, 13.37999999999999012, 10.01041549318726709 ) ) ;
#7707 = ORIENTED_EDGE ( 'NONE', *, *, #9339, .T. ) ;
#7708 = CARTESIAN_POINT ( 'NONE',  ( -3.636496289402153081, 56.32999999999999829, -11.19198476289190936 ) ) ;
#7709 = CARTESIAN_POINT ( 'NONE',  ( 4.711679271994909435, -3.121874999999992184, -11.37499999999960387 ) ) ;
#7710 = CARTESIAN_POINT ( 'NONE',  ( -11.37499999999960387, -90.53437499999978400, -4.711679271994911211 ) ) ;
#7711 = CARTESIAN_POINT ( 'NONE',  ( -13.49999999999999822, -1.220000000000006413, -4.386415899144240349 ) ) ;
#7712 = CARTESIAN_POINT ( 'NONE',  ( 8.593253602144370618, 75.85007813313070812, -10.41182175112990294 ) ) ;
#7713 = CARTESIAN_POINT ( 'NONE',  ( 13.16986379960055054, -85.33124999999978400, -13.16986379959834430 ) ) ;
#7714 = CARTESIAN_POINT ( 'NONE',  ( 0.8232864874221478280, 65.70960053299302217, 13.47579076975969059 ) ) ;
#7715 = CARTESIAN_POINT ( 'NONE',  ( 8.343458848123578520, 68.98000000000000398, 11.48378591275254124 ) ) ;
#7716 = CARTESIAN_POINT ( 'NONE',  ( -3.636496289402153081, 50.32999999999999829, -11.19198476289190936 ) ) ;
#7717 = CARTESIAN_POINT ( 'NONE',  ( 4.171729424061789260, 6.830000000000002736, 12.83926296998457239 ) ) ;
#7718 = CIRCLE ( 'NONE', #8285, 26.00000000000000355 ) ;
#7719 = CARTESIAN_POINT ( 'NONE',  ( -11.48516908419409432, 59.19542272029885766, 7.107131117762169659 ) ) ;
#7720 = CARTESIAN_POINT ( 'NONE',  ( 10.21623194528608458, 45.09073215856821548, 8.828689258619535352 ) ) ;
#7721 = CARTESIAN_POINT ( 'NONE',  ( 12.89448783432755796, 69.57384785835293428, -4.011012806986094859 ) ) ;
#7722 = CARTESIAN_POINT ( 'NONE',  ( -1.900613283885286720, 6.390856018535460592, -12.00000000000297007 ) ) ;
#7723 = CARTESIAN_POINT ( 'NONE',  ( 12.36279736334451052, 30.62854102080525465, -5.439322983125138400 ) ) ;
#7724 = CARTESIAN_POINT ( 'NONE',  ( -12.03366613076771330, 55.70437945554667891, -6.119706988989864982 ) ) ;
#7725 = CARTESIAN_POINT ( 'NONE',  ( -13.38202365434617924, 49.99395983722415338, 1.829691088066569771 ) ) ;
#7726 = CARTESIAN_POINT ( 'NONE',  ( 5.480047553734324062, 63.98142194296197260, -12.33786472815376456 ) ) ;
#7727 = CARTESIAN_POINT ( 'NONE',  ( 13.01599110912158608, 42.55788555145221608, -3.582463918765408373 ) ) ;
#7728 = CARTESIAN_POINT ( 'NONE',  ( 12.79213715724993072, 39.27444083374449946, 4.317700622619438988 ) ) ;
#7729 = ORIENTED_EDGE ( 'NONE', *, *, #9920, .F. ) ;
#7730 = CARTESIAN_POINT ( 'NONE',  ( -7.516515514640333073, 70.46163409174739911, -11.21472715495389139 ) ) ;
#7731 = CARTESIAN_POINT ( 'NONE',  ( -12.79841870162076134, 61.77472664241843603, -4.318434748836910586 ) ) ;
#7732 = CARTESIAN_POINT ( 'NONE',  ( -11.76794919243112325, 4.080000000000008065, 3.823638476888994386 ) ) ;
#7733 = VERTEX_POINT ( 'NONE', #2553 ) ;
#7734 = CARTESIAN_POINT ( 'NONE',  ( -10.27255720726481591, 40.59369077641002832, -8.759258848260193631 ) ) ;
#7735 = ORIENTED_EDGE ( 'NONE', *, *, #11716, .F. ) ;
#7736 = CARTESIAN_POINT ( 'NONE',  ( -13.50000000000000000, 25.93000000000000682, -3.469446951953614189E-15 ) ) ;
#7737 = CARTESIAN_POINT ( 'NONE',  ( -13.16986379960055231, -93.65624999999977263, 13.16986379959834252 ) ) ;
#7738 = EDGE_CURVE ( 'NONE', #10449, #5905, #6195, .T. ) ;
#7739 = CARTESIAN_POINT ( 'NONE',  ( -7.291143994141260196E-08, 47.67999796853253258, 13.49999999999999822 ) ) ;
#7740 = CARTESIAN_POINT ( 'NONE',  ( 1.744899927265306738, 58.11728114404964174, -13.38849203301896651 ) ) ;
#7741 = CARTESIAN_POINT ( 'NONE',  ( 12.17625345903434386, 78.64407479153155123, -5.830030459730453529 ) ) ;
#7742 = CARTESIAN_POINT ( 'NONE',  ( -11.76794919243112325, 74.92999999999999261, -2.882316262207890869E-15 ) ) ;
#7743 = CARTESIAN_POINT ( 'NONE',  ( 12.05296456974564379, -3.033844236144862430E-15, -3.524706777039052330 ) ) ;
#7744 = DIRECTION ( 'NONE',  ( 0.000000000000000000, -1.000000000000000000, 0.000000000000000000 ) ) ;
#7745 = PRODUCT_DEFINITION_CONTEXT ( 'detailed design', #4161, 'design' ) ;
#7746 = CARTESIAN_POINT ( 'NONE',  ( 6.601226367162849940, -99.99999999999998579, 10.86885066916123321 ) ) ;
#7747 = CARTESIAN_POINT ( 'NONE',  ( 2.445080149700053643E-15, 33.17999999999999261, -13.50000000000000000 ) ) ;
#7748 = CARTESIAN_POINT ( 'NONE',  ( 8.043339635997654113, -18.73124999999995666, -8.043339635996304082 ) ) ;
#7749 = CYLINDRICAL_SURFACE ( 'NONE', #3281, 2.000000000000001776 ) ;
#7750 = CIRCLE ( 'NONE', #11414, 8.999999999999998224 ) ;
#7751 = CARTESIAN_POINT ( 'NONE',  ( 3.850668321557367602, 34.04163834952560563, -12.93976093828572616 ) ) ;
#7752 = CARTESIAN_POINT ( 'NONE',  ( -13.49747450356258227, 73.94233775771490969, 0.3603895268416468789 ) ) ;
#7753 = ORIENTED_EDGE ( 'NONE', *, *, #7763, .T. ) ;
#7754 = VERTEX_POINT ( 'NONE', #5503 ) ;
#7755 = DIRECTION ( 'NONE',  ( 0.4999999999999946154, 0.000000000000000000, 0.8660254037844418162 ) ) ;
#7756 = ORIENTED_EDGE ( 'NONE', *, *, #11157, .F. ) ;
#7757 = CARTESIAN_POINT ( 'NONE',  ( -10.92172942406179104, 14.23000000000001997, 7.935100905948385908 ) ) ;
#7758 = CARTESIAN_POINT ( 'NONE',  ( 11.76794919243112325, -12.71999999999999886, 3.823638476888996163 ) ) ;
#7759 = CARTESIAN_POINT ( 'NONE',  ( 11.37499999999960210, -98.85937499999975842, 4.711679271994918317 ) ) ;
#7760 = CARTESIAN_POINT ( 'NONE',  ( -4.525246487782226268, 44.51717099873670946, 12.71929788871430844 ) ) ;
#7761 = FACE_OUTER_BOUND ( 'NONE', #838, .T. ) ;
#7762 = DIRECTION ( 'NONE',  ( -0.000000000000000000, 1.000000000000000000, -0.000000000000000000 ) ) ;
#7763 = EDGE_CURVE ( 'NONE', #13217, #12592, #9879, .T. ) ;
#7764 = CARTESIAN_POINT ( 'NONE',  ( 7.500000000000000888, 98.93000000000002103, 1.224646799147353059E-15 ) ) ;
#7765 = B_SPLINE_CURVE_WITH_KNOTS ( 'NONE', 3,
 ( #14411, #14242, #16904, #15735 ),
 .UNSPECIFIED., .F., .F.,
 ( 4, 4 ),
 ( 0.008723199174958473981, 0.01636875612029862689 ),
 .UNSPECIFIED. ) ;
#7766 = CARTESIAN_POINT ( 'NONE',  ( 12.85627864483936023, 66.57813439057589733, -4.122644307487381532 ) ) ;
#7767 = CARTESIAN_POINT ( 'NONE',  ( 4.171729424061791924, 52.03000000000000114, -12.83926296998457239 ) ) ;
#7768 = CARTESIAN_POINT ( 'NONE',  ( -11.83475973592285513, 71.17061926079419720, 6.495264808528300904 ) ) ;
#7769 = FILL_AREA_STYLE_COLOUR ( '', #13153 ) ;
#7770 = CARTESIAN_POINT ( 'NONE',  ( 18.62500000000000000, -99.89999999999976410, 1.560692158462880521E-12 ) ) ;
#7771 = CARTESIAN_POINT ( 'NONE',  ( 1.898107115681752832, 68.74824965014141753, 13.36594710483466741 ) ) ;
#7772 = CARTESIAN_POINT ( 'NONE',  ( -18.62500000000064659, -75.96562499999980389, 7.714727599197335195 ) ) ;
#7773 = CARTESIAN_POINT ( 'NONE',  ( 4.982188148456265786, 55.00030919837298882, -12.54727938898756534 ) ) ;
#7774 = CARTESIAN_POINT ( 'NONE',  ( -7.714727599200467800, -61.39687499999984510, 18.62499999999934630 ) ) ;
#7775 = CARTESIAN_POINT ( 'NONE',  ( -7.868944743446579793, 65.38296008073473331, 10.97062159917515345 ) ) ;
#7776 = CARTESIAN_POINT ( 'NONE',  ( -7.373414840961570960, 62.40459273648136929, 11.31939194178672814 ) ) ;
#7777 = CARTESIAN_POINT ( 'NONE',  ( -9.387694602222815377, 35.31196052404588670, 9.701610092094997029 ) ) ;
#7778 = CARTESIAN_POINT ( 'NONE',  ( 13.49999999999999822, 19.27999999999999048, 4.386415899144237684 ) ) ;
#7779 = ORIENTED_EDGE ( 'NONE', *, *, #5305, .T. ) ;
#7780 = FACE_OUTER_BOUND ( 'NONE', #11027, .T. ) ;
#7781 = ADVANCED_FACE ( 'NONE', ( #16078 ), #11552, .T. ) ;
#7782 = CARTESIAN_POINT ( 'NONE',  ( -13.35193275233298138, 31.99983217731938012, 1.993971145068321293 ) ) ;
#7783 = CARTESIAN_POINT ( 'NONE',  ( 0.5206494563258732278, 73.16127936737596826, -13.48995723633962207 ) ) ;
#7784 = CARTESIAN_POINT ( 'NONE',  ( 8.660314696132404677, 60.01309689425234239, 10.35850926495430002 ) ) ;
#7785 = CARTESIAN_POINT ( 'NONE',  ( -13.50000000000000000, -9.070000000000002061, -3.469446951953614189E-15 ) ) ;
#7786 = CARTESIAN_POINT ( 'NONE',  ( -3.829800477185295815, 53.54229456450769220, 12.94543166439263082 ) ) ;
#7787 = CARTESIAN_POINT ( 'NONE',  ( 9.520470885617717371, 61.72999999999999687, -6.917026985038131848 ) ) ;
#7788 = CONTEXT_DEPENDENT_SHAPE_REPRESENTATION ( #8706, #5224 ) ;
#7789 = CARTESIAN_POINT ( 'NONE',  ( 2.607531440858944223E-15, 78.18000000000000682, -14.19474002721660355 ) ) ;
#7790 = CARTESIAN_POINT ( 'NONE',  ( 13.40849521964058333, 51.37530757315951746, 1.569414197331337135 ) ) ;
#7791 = CARTESIAN_POINT ( 'NONE',  ( -13.43247398786117230, 37.88223963647511283, -1.378765868932373406 ) ) ;
#7792 = CARTESIAN_POINT ( 'NONE',  ( 13.48777555382222815, 36.44979078757540236, -0.5747704346103513773 ) ) ;
#7793 = CARTESIAN_POINT ( 'NONE',  ( 4.711679271993006957, -37.42812499999992326, 11.37500000000039257 ) ) ;
#7794 = CARTESIAN_POINT ( 'NONE',  ( -1.245489582415950203, 74.63522726745355840, 13.44493988206992441 ) ) ;
#7795 = VECTOR ( 'NONE', #1068, 1000.000000000000000 ) ;
#7796 = CARTESIAN_POINT ( 'NONE',  ( -7.500000000000000000, 108.9300000000000068, -12.00000000000000178 ) ) ;
#7797 = CARTESIAN_POINT ( 'NONE',  ( -1.443680002102475823, 80.62806861202990660, 13.42304612100068262 ) ) ;
#7798 = CARTESIAN_POINT ( 'NONE',  ( 7.500000000000001776, 108.6662573213694856, -2.063574628993714466 ) ) ;
#7799 = VERTEX_POINT ( 'NONE', #17330 ) ;
#7800 = CARTESIAN_POINT ( 'NONE',  ( 2.279995255611139653E-15, 12.17999999999999972, -12.37355403259654985 ) ) ;
#7801 = VERTEX_POINT ( 'NONE', #13435 ) ;
#7802 = CARTESIAN_POINT ( 'NONE',  ( 7.272992578804308828, 60.97999999999999687, 10.01041549318726886 ) ) ;
#7803 = CARTESIAN_POINT ( 'NONE',  ( -4.711679271993003404, -81.20312499999978684, -11.37500000000039613 ) ) ;
#7804 = LINE ( 'NONE', #5054, #6832 ) ;
#7805 = CARTESIAN_POINT ( 'NONE',  ( -8.549982208541774191E-16, 2.680000000000008153, 14.19474002721660355 ) ) ;
#7806 = CARTESIAN_POINT ( 'NONE',  ( 4.683166727831639342, 76.01126718398232640, -12.67683038080413205 ) ) ;
#7807 = CYLINDRICAL_SURFACE ( 'NONE', #1740, 13.50000000000000000 ) ;
#7808 = CARTESIAN_POINT ( 'NONE',  ( -13.49999999999999822, 70.78000000000000114, -4.386415899144240349 ) ) ;
#7809 = CARTESIAN_POINT ( 'NONE',  ( 3.636496289402157078, 44.03000000000000114, -11.19198476289190936 ) ) ;
#7810 = CARTESIAN_POINT ( 'NONE',  ( 6.750022862106053623, 30.42926176209967792, 11.69132975161703669 ) ) ;
#7811 = CARTESIAN_POINT ( 'NONE',  ( -9.960320236238985103, 59.28285562016890964, 9.112740665185853572 ) ) ;
#7812 = CARTESIAN_POINT ( 'NONE',  ( 13.06318910310979398, 45.30856193264118303, 3.408955850317910485 ) ) ;
#7813 = CARTESIAN_POINT ( 'NONE',  ( 13.41584005935412982, 69.37759815817189235, 1.505070243511359207 ) ) ;
#7814 = CARTESIAN_POINT ( 'NONE',  ( 5.606696772960964026, 80.88329787685947281, 12.29363097722763953 ) ) ;
#7815 = CARTESIAN_POINT ( 'NONE',  ( 13.29343906038742240, 30.34724986304589223, 2.352712674252016356 ) ) ;
#7816 = EDGE_CURVE ( 'NONE', #4526, #11897, #11559, .T. ) ;
#7817 = CARTESIAN_POINT ( 'NONE',  ( -6.971261592005899566, 55.43845261729841667, -11.56146040202950864 ) ) ;
#7818 = CARTESIAN_POINT ( 'NONE',  ( -13.48137232301679767, 49.90553325806488516, -0.7090744274153022442 ) ) ;
#7819 = CARTESIAN_POINT ( 'NONE',  ( 7.823624482728693152, 63.88493689099392014, -11.00187558684504729 ) ) ;
#7820 = CARTESIAN_POINT ( 'NONE',  ( 9.806806863896056825, 42.79088325685976457, -9.280060988516410703 ) ) ;
#7821 = CARTESIAN_POINT ( 'NONE',  ( 11.17315624111993344, 39.14503853878225215, 7.577034674267142833 ) ) ;
#7822 = EDGE_LOOP ( 'NONE', ( #8256, #15020, #5141, #1272 ) ) ;
#7823 = CARTESIAN_POINT ( 'NONE',  ( -12.53540363503289967, 70.74778265195330107, -5.016157258731891666 ) ) ;
#7824 = CARTESIAN_POINT ( 'NONE',  ( -6.468465248468677764, 61.41772682254438109, -11.85174451472239987 ) ) ;
#7825 = AXIS2_PLACEMENT_3D ( 'NONE', #7796, #17049, #3529 ) ;
#7826 = CARTESIAN_POINT ( 'NONE',  ( -11.76794919243112325, 6.779999999999995808, -3.823638476888998827 ) ) ;
#7827 = ORIENTED_EDGE ( 'NONE', *, *, #183, .T. ) ;
#7828 = ORIENTED_EDGE ( 'NONE', *, *, #911, .T. ) ;
#7829 = CARTESIAN_POINT ( 'NONE',  ( 13.16986379960055054, -85.33124999999978400, -13.16986379959834430 ) ) ;
#7830 = CARTESIAN_POINT ( 'NONE',  ( 3.401931530595172948, 47.80226563792746219, 13.06448585452245048 ) ) ;
#7831 = CARTESIAN_POINT ( 'NONE',  ( 13.49968223111125987, 57.43320969734387660, -0.09375648845182017743 ) ) ;
#7832 = CARTESIAN_POINT ( 'NONE',  ( -7.272992578804307939, 68.48000000000000398, -10.01041549318726886 ) ) ;
#7833 = CARTESIAN_POINT ( 'NONE',  ( 11.76794919243112325, 79.28000000000001535, 3.823638476888996607 ) ) ;
#7834 = DIRECTION ( 'NONE',  ( 0.000000000000000000, -1.000000000000000000, 0.000000000000000000 ) ) ;
#7835 = AXIS2_PLACEMENT_3D ( 'NONE', #10404, #15761, #2327 ) ;
#7836 = CYLINDRICAL_SURFACE ( 'NONE', #8838, 13.50000000000000000 ) ;
#7837 = CARTESIAN_POINT ( 'NONE',  ( -8.043339635996304082, -82.24374999999977831, -8.043339635997652337 ) ) ;
#7838 = CARTESIAN_POINT ( 'NONE',  ( -19.29752010712865129, 5.918584287042170544, 17.42428528562837542 ) ) ;
#7839 = CARTESIAN_POINT ( 'NONE',  ( 4.929499733297499908, 34.00225962392094914, -12.56974289013172275 ) ) ;
#7840 = CARTESIAN_POINT ( 'NONE',  ( -2.303000823595952262, 73.26280741842690247, -13.30211301100326970 ) ) ;
#7841 = ORIENTED_EDGE ( 'NONE', *, *, #8720, .F. ) ;
#7842 = VERTEX_POINT ( 'NONE', #2817 ) ;
#7843 = CARTESIAN_POINT ( 'NONE',  ( 2.272985001014427393E-15, 80.18000000000002103, -12.37355403259654807 ) ) ;
#7844 = ORIENTED_EDGE ( 'NONE', *, *, #16200, .T. ) ;
#7845 = CARTESIAN_POINT ( 'NONE',  ( 18.62500000000064659, -8.290625000000000355, -7.714727599197336083 ) ) ;
#7846 = CARTESIAN_POINT ( 'NONE',  ( -9.386590952217790829, 44.31237695230070983, 9.713897901698546278 ) ) ;
#7847 = CARTESIAN_POINT ( 'NONE',  ( -7.499999999999998224, -25.82389322351430039, 7.532295102519082519 ) ) ;
#7848 = CARTESIAN_POINT ( 'NONE',  ( 12.75591148537818142, 66.58942501576625261, -4.420261642715005657 ) ) ;
#7849 = CARTESIAN_POINT ( 'NONE',  ( -10.92172942406178926, 49.62999999999999545, -7.935100905948389460 ) ) ;
#7850 = CARTESIAN_POINT ( 'NONE',  ( -11.81742131952455210, 71.17185724881636588, 6.526822490041712221 ) ) ;
#7851 = CARTESIAN_POINT ( 'NONE',  ( 18.62500000000000000, -83.24999999999980105, 1.560692158462880521E-12 ) ) ;
#7852 = CARTESIAN_POINT ( 'NONE',  ( -11.71143577085923049, 68.17956492373299682, 6.715245685198016012 ) ) ;
#7853 = CARTESIAN_POINT ( 'NONE',  ( -13.16986379959834252, 1.006250000000015854, -13.16986379960055409 ) ) ;
#7854 = ADVANCED_FACE ( 'NONE', ( #189 ), #5595, .F. ) ;
#7855 = CARTESIAN_POINT ( 'NONE',  ( 10.10871875307872791, 54.77537364579058021, -8.963922330543132588 ) ) ;
#7856 = CARTESIAN_POINT ( 'NONE',  ( 3.636496289402157078, 18.03000000000001890, -11.19198476289190936 ) ) ;
#7857 = DIRECTION ( 'NONE',  ( 0.000000000000000000, 0.000000000000000000, -1.000000000000000000 ) ) ;
#7858 = CARTESIAN_POINT ( 'NONE',  ( -9.838551016974426133, 65.28917364825832692, 9.244084696182136796 ) ) ;
#7859 = CARTESIAN_POINT ( 'NONE',  ( -0.8900008408070171351, 35.64814624292192491, 13.47797923260558406 ) ) ;
#7860 = CARTESIAN_POINT ( 'NONE',  ( -13.50000000000000000, 20.93000000000000327, -3.469446951953614189E-15 ) ) ;
#7861 = VERTEX_POINT ( 'NONE', #4692 ) ;
#7862 = CARTESIAN_POINT ( 'NONE',  ( -1.328658795546723038E-07, 9.679996299052479714, 13.49999999999999822 ) ) ;
#7863 = CYLINDRICAL_SURFACE ( 'NONE', #13970, 5.000000000000000000 ) ;
#7864 = CARTESIAN_POINT ( 'NONE',  ( 11.76794919243112325, 29.28000000000001180, 3.823638476888996163 ) ) ;
#7865 = CARTESIAN_POINT ( 'NONE',  ( -13.38778841787257967, 31.99111624269271914, 1.750747606360489872 ) ) ;
#7866 = CARTESIAN_POINT ( 'NONE',  ( 0.6169822239420026389, 73.15781583020579149, -13.48596981513675885 ) ) ;
#7867 = CARTESIAN_POINT ( 'NONE',  ( 13.43413273411696984, 60.37283339418769401, 1.647395493114142351 ) ) ;
#7868 = CARTESIAN_POINT ( 'NONE',  ( -8.796156758802018416, 53.34094639218631073, 10.25032176464773670 ) ) ;
#7869 = CARTESIAN_POINT ( 'NONE',  ( 11.76794919243112325, 58.42999999999999261, 1.441158131103945434E-15 ) ) ;
#7870 = CARTESIAN_POINT ( 'NONE',  ( 10.29002516399447664, 51.09446916187894061, 8.745445847329625266 ) ) ;
#7871 = AXIS2_PLACEMENT_3D ( 'NONE', #12711, #2163, #16764 ) ;
#7872 = CARTESIAN_POINT ( 'NONE',  ( -12.50081041153300809, 37.74404765314170618, -5.115235228920670174 ) ) ;
#7873 = CARTESIAN_POINT ( 'NONE',  ( 11.09743137222288567, 36.14041904309804210, 7.687522710969313167 ) ) ;
#7874 = CARTESIAN_POINT ( 'NONE',  ( -4.711679271993001628, -29.10312499999994884, -11.37500000000039613 ) ) ;
#7875 = CARTESIAN_POINT ( 'NONE',  ( -0.5868455399888620194, 74.65889916526552383, 13.48724515689395709 ) ) ;
#7876 = CARTESIAN_POINT ( 'NONE',  ( -7.867229263053499011, 77.38331958151701429, 10.97973947346444312 ) ) ;
#7877 = CARTESIAN_POINT ( 'NONE',  ( -12.21983403303726412, 80.14045539099613791, 5.738378725442176531 ) ) ;
#7878 = CARTESIAN_POINT ( 'NONE',  ( 7.500000000000000000, 108.7258046340738247, -1.043242051446488183 ) ) ;
#7879 = ORIENTED_EDGE ( 'NONE', *, *, #12638, .F. ) ;
#7880 = CARTESIAN_POINT ( 'NONE',  ( 0.000000000000000000, 0.000000000000000000, 0.000000000000000000 ) ) ;
#7881 = CARTESIAN_POINT ( 'NONE',  ( -7.272992578804307939, 3.479999999999997762, -10.01041549318726886 ) ) ;
#7882 = ORIENTED_EDGE ( 'NONE', *, *, #15463, .T. ) ;
#7883 = CARTESIAN_POINT ( 'NONE',  ( -11.76794919243112325, 53.92999999999999972, -2.882316262207890869E-15 ) ) ;
#7884 = CARTESIAN_POINT ( 'NONE',  ( -4.711679271993004292, -5.203124999999986677, -11.37500000000039435 ) ) ;
#7885 = CARTESIAN_POINT ( 'NONE',  ( 3.785595641572113985E-06, 49.17999986388394973, -13.49999999999946887 ) ) ;
#7886 = CARTESIAN_POINT ( 'NONE',  ( 13.49999999999999822, -8.720000000000002416, 4.386415899144237684 ) ) ;
#7887 = CARTESIAN_POINT ( 'NONE',  ( 10.53320440394615787, 75.75205876548513118, -8.444065835725185210 ) ) ;
#7888 = AXIS2_PLACEMENT_3D ( 'NONE', #918, #10222, #15662 ) ;
#7889 = CARTESIAN_POINT ( 'NONE',  ( 8.343458848123583849, 32.88000000000000256, -11.48378591275253768 ) ) ;
#7890 = CARTESIAN_POINT ( 'NONE',  ( 2.607531440858944223E-15, 76.18000000000000682, -14.19474002721660355 ) ) ;
#7891 = CARTESIAN_POINT ( 'NONE',  ( -7.272992578804307939, 38.47999999999999687, -10.01041549318726886 ) ) ;
#7892 = DIRECTION ( 'NONE',  ( -3.552713678800500929E-15, 0.000000000000000000, -1.000000000000000000 ) ) ;
#7893 = CARTESIAN_POINT ( 'NONE',  ( -8.783995296284150101, 58.51886061770396452, -10.25141294735016473 ) ) ;
#7894 = CARTESIAN_POINT ( 'NONE',  ( 8.830119991140810143, 45.02099320959101902, 10.21491743141267250 ) ) ;
#7895 = CARTESIAN_POINT ( 'NONE',  ( 10.17242564541387573, 69.77167130980720344, -8.875356370481091162 ) ) ;
#7896 = EDGE_CURVE ( 'NONE', #5186, #4213, #5941, .T. ) ;
#7897 = CARTESIAN_POINT ( 'NONE',  ( -2.138189944381236884, 66.25688142232024802, -13.50000000000000000 ) ) ;
#7898 = CARTESIAN_POINT ( 'NONE',  ( 1.469576158976823947E-15, 80.93000000000000682, 12.00000000000000178 ) ) ;
#7899 = AXIS2_PLACEMENT_3D ( 'NONE', #11137, #174, #9912 ) ;
#7900 = CARTESIAN_POINT ( 'NONE',  ( -3.266778053494848510, 55.29741596993616781, -13.10567149089917294 ) ) ;
#7901 = CARTESIAN_POINT ( 'NONE',  ( -12.61725017451394137, 50.10401918287165302, 4.802055765613469696 ) ) ;
#7902 = CARTESIAN_POINT ( 'NONE',  ( 12.92176334759158607, 63.28989646019751802, 3.909127044249662841 ) ) ;
#7903 = CARTESIAN_POINT ( 'NONE',  ( 11.58099081591013402, 42.68941737403753223, -6.962115988610442230 ) ) ;
#7904 = CARTESIAN_POINT ( 'NONE',  ( 13.27807327384993918, 39.34399554834261892, 2.441573368172686553 ) ) ;
#7905 = ORIENTED_EDGE ( 'NONE', *, *, #13634, .T. ) ;
#7906 = CARTESIAN_POINT ( 'NONE',  ( -5.200545543539695892, 70.36798564403922285, -12.45811891570486907 ) ) ;
#7907 = CARTESIAN_POINT ( 'NONE',  ( -4.019890708354314945, 61.32453985535606478, -12.88763352006148466 ) ) ;
#7908 = CARTESIAN_POINT ( 'NONE',  ( 7.272992578804311492, 8.880000000000000782, -10.01041549318726709 ) ) ;
#7909 = ORIENTED_EDGE ( 'NONE', *, *, #4495, .T. ) ;
#7910 = ORIENTED_EDGE ( 'NONE', *, *, #5848, .T. ) ;
#7911 = CARTESIAN_POINT ( 'NONE',  ( -4.171729424061791036, 23.52999999999999403, 12.83926296998457239 ) ) ;
#7912 = CARTESIAN_POINT ( 'NONE',  ( -18.62500000000000000, -74.92499999999982663, -1.562973063126292555E-12 ) ) ;
#7913 = CARTESIAN_POINT ( 'NONE',  ( 3.073068557420711056, 61.06950378709134952, -13.14558087420024712 ) ) ;
#7914 = CARTESIAN_POINT ( 'NONE',  ( 9.703214173663569753, 72.06388277513445928, 9.386303311651374770 ) ) ;
#7915 = CARTESIAN_POINT ( 'NONE',  ( 13.39493254271660128, 57.37134799861901513, 1.681008321832105468 ) ) ;
#7916 = ADVANCED_FACE ( 'NONE', ( #14127 ), #5857, .T. ) ;
#7917 = CARTESIAN_POINT ( 'NONE',  ( 7.272992578804311492, 70.87999999999998124, -10.01041549318726709 ) ) ;
#7918 = CARTESIAN_POINT ( 'NONE',  ( -11.76794919243112325, 74.92999999999999261, -2.882316262207890869E-15 ) ) ;
#7919 = CARTESIAN_POINT ( 'NONE',  ( -1.404360861943162231, 47.62954975977737604, 13.42896419968065658 ) ) ;
#7920 = CARTESIAN_POINT ( 'NONE',  ( 6.303891475472711114, -100.0000000000000568, 15.41241088168433926 ) ) ;
#7921 = CARTESIAN_POINT ( 'NONE',  ( -4.171729424061787483, 75.33000000000001251, -12.83926296998457417 ) ) ;
#7922 = CARTESIAN_POINT ( 'NONE',  ( 11.37500000000039435, -17.69062499999995453, -4.711679271993004292 ) ) ;
#7923 = CARTESIAN_POINT ( 'NONE',  ( 2.138189944381200469, 45.10311857767973720, -13.50000000000001421 ) ) ;
#7924 = CARTESIAN_POINT ( 'NONE',  ( 10.15193879533094545, 33.77277897302748499, -8.899270537352469645 ) ) ;
#7925 = CARTESIAN_POINT ( 'NONE',  ( -7.690819183321357499, 73.46921467895631963, -11.09564406485981003 ) ) ;
#7926 = ORIENTED_EDGE ( 'NONE', *, *, #6694, .F. ) ;
#7927 = ORIENTED_EDGE ( 'NONE', *, *, #9880, .F. ) ;
#7928 = CARTESIAN_POINT ( 'NONE',  ( 11.76794919243112680, 76.57999999999998408, -3.823638476888993942 ) ) ;
#7929 = ORIENTED_EDGE ( 'NONE', *, *, #3866, .F. ) ;
#7930 = CARTESIAN_POINT ( 'NONE',  ( -9.552639591052204498E-13, -86.33749999999982094, 11.37499999999999645 ) ) ;
#7931 = CARTESIAN_POINT ( 'NONE',  ( -10.11920711176065701, 44.27449785737638166, 8.935975526465597341 ) ) ;
#7932 = CARTESIAN_POINT ( 'NONE',  ( 10.69176227072922281, 7.854010657973331533, 15.43600950528676385 ) ) ;
#7933 = CARTESIAN_POINT ( 'NONE',  ( 10.70226043262125870, 66.74271198536885663, -8.240297481720242345 ) ) ;
#7934 = EDGE_CURVE ( 'NONE', #11444, #9328, #12958, .T. ) ;
#7935 = CARTESIAN_POINT ( 'NONE',  ( 13.50000000000000355, 45.57999999999998408, -4.386415899144233244 ) ) ;
#7936 = CARTESIAN_POINT ( 'NONE',  ( -8.912460682575348514, 71.33536275098259694, 10.15239226002055517 ) ) ;
#7937 = VECTOR ( 'NONE', #8508, 1000.000000000000000 ) ;
#7938 = CARTESIAN_POINT ( 'NONE',  ( 18.62500000000064304, -50.99062499999987352, -7.714727599197335195 ) ) ;
#7939 = CARTESIAN_POINT ( 'NONE',  ( -12.85088929819618109, 67.78133704544254101, -4.136414102390641112 ) ) ;
#7940 = CARTESIAN_POINT ( 'NONE',  ( 18.62499999999935341, -25.00937499999992397, 7.714727599200469577 ) ) ;
#7941 = CARTESIAN_POINT ( 'NONE',  ( 10.52332088831184720, 54.75260603147985705, -8.456359092437114811 ) ) ;
#7942 = CARTESIAN_POINT ( 'NONE',  ( 18.62499999999934630, -82.20937499999980957, 7.714727599200467800 ) ) ;
#7943 = CARTESIAN_POINT ( 'NONE',  ( -12.70587675808030070, 65.09482543421927403, 4.561926965439528914 ) ) ;
#7944 = CARTESIAN_POINT ( 'NONE',  ( -9.395184304882585380, 35.31158635481718022, 9.694355262636014103 ) ) ;
#7945 = CARTESIAN_POINT ( 'NONE',  ( -13.49999999999999822, 18.08000000000000185, 4.386415899144235908 ) ) ;
#7946 = ORIENTED_EDGE ( 'NONE', *, *, #13536, .T. ) ;
#7947 = CYLINDRICAL_SURFACE ( 'NONE', #17163, 13.50000000000000000 ) ;
#7948 = DIRECTION ( 'NONE',  ( -0.000000000000000000, -1.000000000000000000, -0.000000000000000000 ) ) ;
#7949 = CARTESIAN_POINT ( 'NONE',  ( -7.466064059507305117, 31.45946987589979926, -11.24836648485607071 ) ) ;
#7950 = DIRECTION ( 'NONE',  ( 0.000000000000000000, 1.000000000000000000, 0.000000000000000000 ) ) ;
#7951 = CARTESIAN_POINT ( 'NONE',  ( -9.520470885617715595, -11.36999999999999744, -6.917026985038136289 ) ) ;
#7952 = CARTESIAN_POINT ( 'NONE',  ( 3.131229719746321916, 59.79264428906494544, 13.13212888701132997 ) ) ;
#7953 = ADVANCED_FACE ( 'NONE', ( #359 ), #13860, .F. ) ;
#7954 = CARTESIAN_POINT ( 'NONE',  ( -10.92172942406178926, -9.369999999999995666, -7.935100905948389460 ) ) ;
#7955 = CARTESIAN_POINT ( 'NONE',  ( -6.655638788749627111, 53.43463457656628890, 11.74728228429494159 ) ) ;
#7956 = CARTESIAN_POINT ( 'NONE',  ( 11.76794919243112325, 52.43000000000000682, 1.441158131103945434E-15 ) ) ;
#7957 = ITEM_DEFINED_TRANSFORMATION ( 'NONE', 'NONE', #13550,  #16654 ) ;
#7958 = CARTESIAN_POINT ( 'NONE',  ( -8.343458848123582072, 70.37999999999999545, 11.48378591275254124 ) ) ;
#7959 = CARTESIAN_POINT ( 'NONE',  ( 12.72881000398506579, 51.26746853374235258, 4.501197650617609014 ) ) ;
#7960 = CARTESIAN_POINT ( 'NONE',  ( -10.71889181782863254, 37.61765628241656856, -8.218708770179583567 ) ) ;
#7961 = CARTESIAN_POINT ( 'NONE',  ( 13.30455254956636324, 36.34955702229247265, 2.288870851817195184 ) ) ;
#7962 = CARTESIAN_POINT ( 'NONE',  ( 11.37499999999960210, -106.1093749999997584, 4.711679271994916540 ) ) ;
#7963 = CARTESIAN_POINT ( 'NONE',  ( -0.6217783953300516364, 74.65764314461276285, 13.48567423263519771 ) ) ;
#7964 = CARTESIAN_POINT ( 'NONE',  ( -13.50003724147074458, 76.93564051261272141, 0.1657311543569034151 ) ) ;
#7965 = CARTESIAN_POINT ( 'NONE',  ( -12.24434757080924641, 80.13838886078774237, 5.685888707796101116 ) ) ;
#7966 = CARTESIAN_POINT ( 'NONE',  ( -11.76794919243112325, 10.08000000000000718, 3.823638476888994386 ) ) ;
#7967 = CARTESIAN_POINT ( 'NONE',  ( 7.500000000000000000, 107.9345255869306044, -5.560661329642322848 ) ) ;
#7968 = DIRECTION ( 'NONE',  ( -0.000000000000000000, -1.000000000000000000, -0.000000000000000000 ) ) ;
#7969 = CARTESIAN_POINT ( 'NONE',  ( -9.520470885617715595, 3.629999999999994564, -6.917026985038136289 ) ) ;
#7970 = CARTESIAN_POINT ( 'NONE',  ( 2.272985001014427393E-15, 53.17999999999999972, -12.37355403259654807 ) ) ;
#7971 = CARTESIAN_POINT ( 'NONE',  ( -4.711679271994916540, -70.79687499999981526, 11.37499999999960565 ) ) ;
#7972 = CARTESIAN_POINT ( 'NONE',  ( 13.16986379959834075, -31.21874999999992539, 13.16986379960055231 ) ) ;
#7973 = CARTESIAN_POINT ( 'NONE',  ( 13.50000000000000000, -11.56999999999999673, 1.734723475976807094E-15 ) ) ;
#7974 = AXIS2_PLACEMENT_3D ( 'NONE', #11662, #3869, #2606 ) ;
#7975 = CARTESIAN_POINT ( 'NONE',  ( -8.891200544363830713E-16, 34.67999999999999261, 13.50000000000000000 ) ) ;
#7976 = CARTESIAN_POINT ( 'NONE',  ( 10.27537742884199368, 75.76631104229213065, -8.763344131083259825 ) ) ;
#7977 = EDGE_CURVE ( 'NONE', #14800, #13257, #4432, .T. ) ;
#7978 = CARTESIAN_POINT ( 'NONE',  ( 4.171729424061789260, 67.82999999999999829, 12.83926296998457417 ) ) ;
#7979 = CARTESIAN_POINT ( 'NONE',  ( -9.520470885617717371, 36.22999999999999687, 6.917026985038133624 ) ) ;
#7980 = CARTESIAN_POINT ( 'NONE',  ( 1.653273178848926472E-15, 30.93000000000001393, 13.50000000000000000 ) ) ;
#7981 = CARTESIAN_POINT ( 'NONE',  ( -9.718168175322020375, 58.56428136966050602, -9.379168268827697830 ) ) ;
#7982 = CARTESIAN_POINT ( 'NONE',  ( 4.611897008443751389, 44.84600509516975109, 12.68780702028759144 ) ) ;
#7983 = CARTESIAN_POINT ( 'NONE',  ( 13.18589603968220203, 69.53262849552022828, -2.898846619569253047 ) ) ;
#7984 = AXIS2_PLACEMENT_3D ( 'NONE', #5093, #11892, #4013 ) ;
#7985 = DIRECTION ( 'NONE',  ( -0.000000000000000000, 1.000000000000000000, -0.000000000000000000 ) ) ;
#7986 = DIRECTION ( 'NONE',  ( 0.000000000000000000, 1.000000000000000000, 0.000000000000000000 ) ) ;
#7987 = CARTESIAN_POINT ( 'NONE',  ( -0.5738463663737329856, 55.20063339759468590, -13.48779904819468101 ) ) ;
#7988 = CARTESIAN_POINT ( 'NONE',  ( -10.51139941513729958, 49.60641348581317089, -8.476086535629807628 ) ) ;
#7989 = CARTESIAN_POINT ( 'NONE',  ( 13.31815325490439861, 63.50779534182326813, -2.215341855570049479 ) ) ;
#7990 = CARTESIAN_POINT ( 'NONE',  ( 9.372370473719398021, 42.81294516566138952, -9.725257989828588023 ) ) ;
#7991 = CARTESIAN_POINT ( 'NONE',  ( 8.950822057147354016, 39.02672537493957350, 10.10929111056123553 ) ) ;
#7992 = ORIENTED_EDGE ( 'NONE', *, *, #12689, .T. ) ;
#7993 = CARTESIAN_POINT ( 'NONE',  ( -7.766575051535378194, 70.47255142998834287, -11.04220757594332447 ) ) ;
#7994 = CARTESIAN_POINT ( 'NONE',  ( 8.043339635996300530, -14.56874999999996589, 8.043339635997654113 ) ) ;
#7995 = ORIENTED_EDGE ( 'NONE', *, *, #6196, .T. ) ;
#7996 = VERTEX_POINT ( 'NONE', #12473 ) ;
#7997 = CARTESIAN_POINT ( 'NONE',  ( 10.92172942406179104, 18.72999999999999687, -7.935100905948385908 ) ) ;
#7998 = CARTESIAN_POINT ( 'NONE',  ( 18.62500000000000000, -66.59999999999983800, 1.560692158462880521E-12 ) ) ;
#7999 = CARTESIAN_POINT ( 'NONE',  ( 4.736358946727592389, 61.00938531345052240, -12.64187847761339434 ) ) ;
#8000 = CARTESIAN_POINT ( 'NONE',  ( -8.343458848123582072, 15.37999999999999901, 11.48378591275254124 ) ) ;
#8001 = CIRCLE ( 'NONE', #9699, 22.50000000000000355 ) ;
#8002 = EDGE_CURVE ( 'NONE', #12569, #3120, #10097, .T. ) ;
#8003 = CARTESIAN_POINT ( 'NONE',  ( 10.32313480350834389, 72.09643373092249874, 8.701801321890403784 ) ) ;
#8004 = CARTESIAN_POINT ( 'NONE',  ( 12.42105065504388506, 57.62284780083921021, -5.288814127532169174 ) ) ;
#8005 = CARTESIAN_POINT ( 'NONE',  ( -11.76794919243112325, 68.93000000000000682, -2.882316262207890869E-15 ) ) ;
#8006 = CARTESIAN_POINT ( 'NONE',  ( 3.636496289402154414, 72.83000000000001251, 11.19198476289190936 ) ) ;
#8007 = CARTESIAN_POINT ( 'NONE',  ( -9.925988568760681474, 47.28464472409913810, 9.150140798969051303 ) ) ;
#8008 = FACE_OUTER_BOUND ( 'NONE', #15106, .T. ) ;
#8009 = CARTESIAN_POINT ( 'NONE',  ( 3.702617594344294272, -100.0000000000000426, 13.96937958327705864 ) ) ;
#8010 = CARTESIAN_POINT ( 'NONE',  ( -13.49999999999999822, 75.78000000000000114, -4.386415899144240349 ) ) ;
#8011 = CARTESIAN_POINT ( 'NONE',  ( 11.37499999999960210, -15.60937499999996270, 4.711679271994918317 ) ) ;
#8012 = CARTESIAN_POINT ( 'NONE',  ( 4.171729424061791924, 45.03000000000000114, -12.83926296998457239 ) ) ;
#8013 = CARTESIAN_POINT ( 'NONE',  ( 13.47686814967910074, 33.45793751627489598, -0.8093861106240824999 ) ) ;
#8014 = CARTESIAN_POINT ( 'NONE',  ( -9.748234396007397606, 73.56618743211103606, -9.339340668855360406 ) ) ;
#8015 = ORIENTED_EDGE ( 'NONE', *, *, #4516, .T. ) ;
#8016 = ORIENTED_EDGE ( 'NONE', *, *, #3771, .T. ) ;
#8017 = CARTESIAN_POINT ( 'NONE',  ( 7.272992578804308828, 78.97999999999998977, 10.01041549318726886 ) ) ;
#8018 = ORIENTED_EDGE ( 'NONE', *, *, #2551, .F. ) ;
#8019 = CARTESIAN_POINT ( 'NONE',  ( 9.538709233711902776E-13, -61.36249999999986215, -11.37499999999999645 ) ) ;
#8020 = CARTESIAN_POINT ( 'NONE',  ( -8.891200544363830713E-16, 58.67999999999999261, 13.50000000000000000 ) ) ;
#8021 = CARTESIAN_POINT ( 'NONE',  ( 8.022689779262613285, 7.854708479871425730, 16.97418022790854764 ) ) ;
#8022 = CARTESIAN_POINT ( 'NONE',  ( 13.49999999999999822, 39.27999999999999403, 4.386415899144237684 ) ) ;
#8023 = CARTESIAN_POINT ( 'NONE',  ( -6.568958932228524894, 71.43823863022225851, 11.79934775472050212 ) ) ;
#8024 = CARTESIAN_POINT ( 'NONE',  ( -18.62500000000064659, -35.41562499999989200, 7.714727599197333419 ) ) ;
#8025 = CARTESIAN_POINT ( 'NONE',  ( -12.82751988175667357, 67.77861818588846177, -4.208333171070940182 ) ) ;
#8026 = CARTESIAN_POINT ( 'NONE',  ( -13.16986379959834252, -32.29374999999990337, -13.16986379960055409 ) ) ;
#8027 = CARTESIAN_POINT ( 'NONE',  ( 11.54301513894250064, 54.69114107474510433, -7.000628745448283397 ) ) ;
#8028 = CARTESIAN_POINT ( 'NONE',  ( 7.272992578804308828, 16.98000000000000753, 10.01041549318726709 ) ) ;
#8029 = FACE_OUTER_BOUND ( 'NONE', #2194, .T. ) ;
#8030 = EDGE_CURVE ( 'NONE', #15045, #4640, #5660, .T. ) ;
#8031 = CARTESIAN_POINT ( 'NONE',  ( -13.03270642126316048, 64.80436272303023770, -3.522134089092859632 ) ) ;
#8032 = CARTESIAN_POINT ( 'NONE',  ( -11.76794919243112325, 21.77999999999999758, -3.823638476888998827 ) ) ;
#8033 = CARTESIAN_POINT ( 'NONE',  ( -11.83548569472881162, 34.68943475006721400, -6.493960592972081614 ) ) ;
#8034 = ORIENTED_EDGE ( 'NONE', *, *, #2906, .T. ) ;
#8035 = CARTESIAN_POINT ( 'NONE',  ( -1.363343349470708815E-11, 9.313974596216116453, -12.00000000000000355 ) ) ;
#8036 = CARTESIAN_POINT ( 'NONE',  ( -8.357336213632441613, 31.49890460822483362, -10.60832285590191049 ) ) ;
#8037 = CARTESIAN_POINT ( 'NONE',  ( 11.40946131305635802, 72.70018184489865121, -7.219862210453702467 ) ) ;
#8038 = CARTESIAN_POINT ( 'NONE',  ( 11.76794919243112325, -12.71999999999999886, 3.823638476888996163 ) ) ;
#8039 = DIRECTION ( 'NONE',  ( 0.000000000000000000, 0.000000000000000000, -1.000000000000000000 ) ) ;
#8040 = CARTESIAN_POINT ( 'NONE',  ( 4.171729424061789260, -5.170000000000000817, 12.83926296998457239 ) ) ;
#8041 = CARTESIAN_POINT ( 'NONE',  ( -9.666059139767755326, 53.29810990967069273, 9.426597848540740898 ) ) ;
#8042 = CARTESIAN_POINT ( 'NONE',  ( -3.636496289402155746, 48.52999999999999403, 11.19198476289190936 ) ) ;
#8043 = CARTESIAN_POINT ( 'NONE',  ( 4.171729424061791924, 66.03000000000000114, -12.83926296998457239 ) ) ;
#8044 = CARTESIAN_POINT ( 'NONE',  ( 4.957982560739019995, 50.85884492221607189, 12.55662115431407955 ) ) ;
#8045 = CARTESIAN_POINT ( 'NONE',  ( -13.07003727117247038, 37.80950068799819519, -3.384012662600688337 ) ) ;
#8046 = VECTOR ( 'NONE', #14184, 1000.000000000000000 ) ;
#8047 = CARTESIAN_POINT ( 'NONE',  ( 12.63456399010862619, 36.25766377199223456, 4.761015956925509940 ) ) ;
#8048 = CARTESIAN_POINT ( 'NONE',  ( 9.538709233711902776E-13, -94.66249999999979536, -11.37499999999999645 ) ) ;
#8049 = EDGE_CURVE ( 'NONE', #2258, #3134, #13347, .T. ) ;
#8050 = CARTESIAN_POINT ( 'NONE',  ( -7.560656945971843790, 74.39645029488065120, 11.18730623038837280 ) ) ;
#8051 = PRODUCT_DEFINITION_SHAPE ( 'NONE', 'NONE',  #17491 ) ;
#8052 = SHAPE_REPRESENTATION ( 'Nut', ( #16654 ), #11308 ) ;
#8053 = CARTESIAN_POINT ( 'NONE',  ( -13.27243981434447484, 76.84295076259492419, -2.470663295667402171 ) ) ;
#8054 = CARTESIAN_POINT ( 'NONE',  ( -13.15097131915865702, 79.82156063716328731, -3.058016821922826090 ) ) ;
#8055 = CARTESIAN_POINT ( 'NONE',  ( -11.76794919243112325, 12.92999999999999616, -2.602085213965210642E-15 ) ) ;
#8056 = CARTESIAN_POINT ( 'NONE',  ( 7.500000000000000000, 104.6873333394687080, -9.035253535952437076 ) ) ;
#8057 = CARTESIAN_POINT ( 'NONE',  ( -13.49999999999999822, 7.779999999999992255, -4.386415899144240349 ) ) ;
#8058 = CARTESIAN_POINT ( 'NONE',  ( -3.636496289402152637, 3.329999999999999627, -11.19198476289190936 ) ) ;
#8059 = CARTESIAN_POINT ( 'NONE',  ( -9.520470885617717371, 51.22999999999999687, 6.917026985038133624 ) ) ;
#8060 = CARTESIAN_POINT ( 'NONE',  ( -9.552639591052204498E-13, -12.48749999999997051, 11.37500000000000000 ) ) ;
#8061 = CARTESIAN_POINT ( 'NONE',  ( -7.714727599200467800, -44.74687499999989626, 18.62499999999934630 ) ) ;
#8062 = CARTESIAN_POINT ( 'NONE',  ( 10.92172942406178926, -11.86999999999999922, 7.935100905948385908 ) ) ;
#8063 = CARTESIAN_POINT ( 'NONE',  ( -8.070270851187604677, 40.48603366841279438, -10.82230097288300641 ) ) ;
#8064 = CARTESIAN_POINT ( 'NONE',  ( -12.50000000000000000, -18.00000000000000355, -2.204364238465235822E-15 ) ) ;
#8065 = CARTESIAN_POINT ( 'NONE',  ( 5.856966054657046783, 75.96662800222769363, -12.16416065871167262 ) ) ;
#8066 = CARTESIAN_POINT ( 'NONE',  ( 0.000000000000000000, 108.9300000000000068, 6.000000000000001776 ) ) ;
#8067 = CARTESIAN_POINT ( 'NONE',  ( 11.76794919243112325, 37.28000000000000114, 3.823638476888996607 ) ) ;
#8068 = CARTESIAN_POINT ( 'NONE',  ( -9.321700413722924239, 41.31521659627871657, 9.765034796684853191 ) ) ;
#8069 = CARTESIAN_POINT ( 'NONE',  ( -8.798798133082613049, 58.51955967947071713, -10.23870886399114255 ) ) ;
#8070 = DIRECTION ( 'NONE',  ( 0.000000000000000000, 0.000000000000000000, -1.000000000000000000 ) ) ;
#8071 = DIRECTION ( 'NONE',  ( -0.000000000000000000, -1.000000000000000000, -0.000000000000000000 ) ) ;
#8072 = FACE_OUTER_BOUND ( 'NONE', #2365, .T. ) ;
#8073 = CARTESIAN_POINT ( 'NONE',  ( -10.08120899900550427, 55.58349057628856826, -8.978837819965084677 ) ) ;
#8074 = EDGE_CURVE ( 'NONE', #3274, #2674, #5057, .T. ) ;
#8075 = CARTESIAN_POINT ( 'NONE',  ( -12.29411837055197054, 49.72588110055323085, -5.581586529286209242 ) ) ;
#8076 = CARTESIAN_POINT ( 'NONE',  ( 12.94123504964344384, 63.56776154898143005, -3.846256073626998173 ) ) ;
#8077 = CARTESIAN_POINT ( 'NONE',  ( 11.96321250603508624, 42.66099223898741144, -6.255588818712046084 ) ) ;
#8078 = CARTESIAN_POINT ( 'NONE',  ( 11.14178970317686712, 39.14311694041391831, 7.623027801797891634 ) ) ;
#8079 = ORIENTED_EDGE ( 'NONE', *, *, #16100, .F. ) ;
#8080 = CARTESIAN_POINT ( 'NONE',  ( -9.905601374715363505, 70.57426321601532493, -9.172207517655735387 ) ) ;
#8081 = CARTESIAN_POINT ( 'NONE',  ( 12.50000000000000000, -18.00000000000000355, -2.204364238465235822E-15 ) ) ;
#8082 = ORIENTED_EDGE ( 'NONE', *, *, #8935, .F. ) ;
#8083 = ORIENTED_EDGE ( 'NONE', *, *, #17010, .T. ) ;
#8084 = CARTESIAN_POINT ( 'NONE',  ( -13.49999999999999822, 22.77999999999999403, -4.386415899144240349 ) ) ;
#8085 = CARTESIAN_POINT ( 'NONE',  ( -18.62499999999934985, -57.23437499999987921, -7.714727599200458918 ) ) ;
#8086 = CARTESIAN_POINT ( 'NONE',  ( 5.801648381285460232, 60.96920856786400122, -12.20604370177328946 ) ) ;
#8087 = AXIS2_PLACEMENT_3D ( 'NONE', #12633, #10964, #5583 ) ;
#8088 = CARTESIAN_POINT ( 'NONE',  ( -10.92172942406179104, 9.230000000000002203, 7.935100905948385908 ) ) ;
#8089 = DIRECTION ( 'NONE',  ( -0.000000000000000000, -1.000000000000000000, -0.000000000000000000 ) ) ;
#8090 = CARTESIAN_POINT ( 'NONE',  ( 13.49670674025940187, 57.44045678757618845, -0.3048764090252299996 ) ) ;
#8091 = CARTESIAN_POINT ( 'NONE',  ( -7.272992578804310604, 69.38000000000000966, 10.01041549318726709 ) ) ;
#8092 = CARTESIAN_POINT ( 'NONE',  ( -4.171729424061791036, 34.53000000000000114, 12.83926296998457239 ) ) ;
#8093 = CARTESIAN_POINT ( 'NONE',  ( 9.520470885617717371, 79.72999999999998977, -6.917026985038131848 ) ) ;
#8094 = CARTESIAN_POINT ( 'NONE',  ( -9.891620756194170028, 47.28642918340351287, 9.187267813302650410 ) ) ;
#8095 = DIRECTION ( 'NONE',  ( -0.000000000000000000, 1.000000000000000000, -0.000000000000000000 ) ) ;
#8096 = CARTESIAN_POINT ( 'NONE',  ( 13.49999999999999822, 38.27999999999999403, 4.386415899144236796 ) ) ;
#8097 = DIRECTION ( 'NONE',  ( 1.000000000000000000, 8.673617379884037937E-17, 0.000000000000000000 ) ) ;
#8098 = CARTESIAN_POINT ( 'NONE',  ( 8.043339635996300530, -14.56874999999996589, 8.043339635997654113 ) ) ;
#8099 = CIRCLE ( 'NONE', #14544, 9.000000000000000000 ) ;
#8100 = CARTESIAN_POINT ( 'NONE',  ( -2.138189944381236884, 51.25688142232026934, -13.50000000000000000 ) ) ;
#8101 = CARTESIAN_POINT ( 'NONE',  ( 12.93524070685253058, 33.56853690860952355, -3.868045386693336418 ) ) ;
#8102 = CARTESIAN_POINT ( 'NONE',  ( -7.480073533223071891, 73.46007376390073773, -11.23826375466742178 ) ) ;
#8103 = EDGE_LOOP ( 'NONE', ( #925, #12439, #8610, #781 ) ) ;
#8104 = EDGE_LOOP ( 'NONE', ( #12855, #2825, #1102, #8976 ) ) ;
#8105 = CARTESIAN_POINT ( 'NONE',  ( -3.984372987094109586, 62.53673597769582670, 12.89868305420871408 ) ) ;
#8106 = ORIENTED_EDGE ( 'NONE', *, *, #16476, .F. ) ;
#8107 = CARTESIAN_POINT ( 'NONE',  ( -13.32866946258720908, 41.00521990185777810, 2.143963826540092654 ) ) ;
#8108 = CARTESIAN_POINT ( 'NONE',  ( 4.711679271994911211, -60.32187499999988489, -11.37499999999960210 ) ) ;
#8109 = CARTESIAN_POINT ( 'NONE',  ( -0.6445126736188436789, 44.65682569745120389, 13.48462267080572374 ) ) ;
#8110 = CARTESIAN_POINT ( 'NONE',  ( -7.499999999999997335, -25.65291190719446490, 7.723695278929465502 ) ) ;
#8111 = AXIS2_PLACEMENT_3D ( 'NONE', #2756, #9779, #8188 ) ;
#8112 = CARTESIAN_POINT ( 'NONE',  ( -4.171729424061791036, 44.53000000000000114, 12.83926296998457239 ) ) ;
#8113 = CARTESIAN_POINT ( 'NONE',  ( -13.46053110311059342, 70.96573976700906883, 1.032151187161497674 ) ) ;
#8114 = CARTESIAN_POINT ( 'NONE',  ( -18.62500000000000000, -34.37499999999990052, -1.562973063126292757E-12 ) ) ;
#8115 = CARTESIAN_POINT ( 'NONE',  ( -13.32209690758261367, 67.85292585843949098, -2.195106065840739973 ) ) ;
#8116 = CARTESIAN_POINT ( 'NONE',  ( 18.62500000000000000, -9.399999999999959499, 1.560692158462880521E-12 ) ) ;
#8117 = CARTESIAN_POINT ( 'NONE',  ( 13.37361882778371580, 54.49663737476366521, -1.905621438755049413 ) ) ;
#8118 = CARTESIAN_POINT ( 'NONE',  ( -7.272992578804307939, 15.47999999999999865, -10.01041549318726886 ) ) ;
#8119 = FACE_OUTER_BOUND ( 'NONE', #10296, .T. ) ;
#8120 = CARTESIAN_POINT ( 'NONE',  ( -13.40504862348259607, 64.98588083424387207, 1.603266894393355679 ) ) ;
#8121 = CARTESIAN_POINT ( 'NONE',  ( -12.97126758716428796, 35.06420632578307561, 3.750847537641872620 ) ) ;
#8122 = ORIENTED_EDGE ( 'NONE', *, *, #14797, .F. ) ;
#8123 = FACE_OUTER_BOUND ( 'NONE', #17053, .T. ) ;
#8124 = CARTESIAN_POINT ( 'NONE',  ( -7.638144213919573211, 31.46690397426329966, -11.13304072010164170 ) ) ;
#8125 = CARTESIAN_POINT ( 'NONE',  ( 3.487563165784445474, 73.05459837061692951, -13.04193799940900966 ) ) ;
#8126 = CARTESIAN_POINT ( 'NONE',  ( -7.272992578804307939, -11.51999999999999957, -10.01041549318726886 ) ) ;
#8127 = CARTESIAN_POINT ( 'NONE',  ( 3.272115130898746838, 59.79762580205674283, 13.09749008070057918 ) ) ;
#8128 = CARTESIAN_POINT ( 'NONE',  ( -10.92172942406178926, -15.37000000000000099, -7.935100905948389460 ) ) ;
#8129 = CARTESIAN_POINT ( 'NONE',  ( -13.47893375659474025, 52.90398739453420518, -0.7538941320434108251 ) ) ;
#8130 = APPLICATION_CONTEXT ( 'automotive_design' ) ;
#8131 = EDGE_CURVE ( 'NONE', #6426, #1275, #8316, .T. ) ;
#8132 = CARTESIAN_POINT ( 'NONE',  ( -11.76794919243112325, 48.07999999999998408, 3.823638476888994386 ) ) ;
#8133 = CARTESIAN_POINT ( 'NONE',  ( 10.92172942406179104, 65.72999999999998977, -7.935100905948385908 ) ) ;
#8134 = CARTESIAN_POINT ( 'NONE',  ( 4.913540562192366679, 50.85718164286154064, 12.57411717337579482 ) ) ;
#8135 = CARTESIAN_POINT ( 'NONE',  ( -5.826744371414541490, 37.39211206380475971, -12.17872776587915951 ) ) ;
#8136 = CARTESIAN_POINT ( 'NONE',  ( 13.31893752994962199, 36.35261631618632094, 2.203904136930395108 ) ) ;
#8137 = CARTESIAN_POINT ( 'NONE',  ( 4.711679271994911211, -93.62187499999978968, -11.37499999999960210 ) ) ;
#8138 = CARTESIAN_POINT ( 'NONE',  ( -8.133420942632833217, 74.37112280558582711, 10.77516524646321194 ) ) ;
#8139 = CARTESIAN_POINT ( 'NONE',  ( -13.29830443190622802, 76.84825558968388748, -2.324888195045509587 ) ) ;
#8140 = CARTESIAN_POINT ( 'NONE',  ( -12.10733961092197397, 79.71006380404250535, -5.975826969573788894 ) ) ;
#8141 = CARTESIAN_POINT ( 'NONE',  ( -11.76794919243112325, 9.929999999999994387, -2.602085213965210642E-15 ) ) ;
#8142 = DIRECTION ( 'NONE',  ( 0.000000000000000000, -1.000000000000000000, 0.000000000000000000 ) ) ;
#8143 = DIRECTION ( 'NONE',  ( -1.000000000000000000, -0.000000000000000000, -0.000000000000000000 ) ) ;
#8144 = CARTESIAN_POINT ( 'NONE',  ( -7.409984580736203970E-16, -1.320000000000003615, 12.37355403259654985 ) ) ;
#8145 = CARTESIAN_POINT ( 'NONE',  ( -7.576616670048093940E-16, 48.67999999999999261, 12.37355403259654807 ) ) ;
#8146 = CARTESIAN_POINT ( 'NONE',  ( -9.552639591052204498E-13, -62.43749999999985079, 11.37500000000000000 ) ) ;
#8147 = CARTESIAN_POINT ( 'NONE',  ( -18.62499999999934985, -7.284374999999982947, -7.714727599200458918 ) ) ;
#8148 = CARTESIAN_POINT ( 'NONE',  ( -8.343458848123576743, -10.51999999999999780, -11.48378591275254301 ) ) ;
#8149 = CARTESIAN_POINT ( 'NONE',  ( 8.343458848123580296, 34.97999999999998977, 11.48378591275253768 ) ) ;
#8150 = CARTESIAN_POINT ( 'NONE',  ( 11.76865692967993482, 75.18437996510870391, 6.618042598872824200 ) ) ;
#8151 = CARTESIAN_POINT ( 'NONE',  ( -18.62500000000064659, -92.61562499999978115, 7.714727599197333419 ) ) ;
#8152 = CARTESIAN_POINT ( 'NONE',  ( -3.636496289402153081, 41.32999999999999829, -11.19198476289190936 ) ) ;
#8153 = CARTESIAN_POINT ( 'NONE',  ( -11.42231603963109521, 41.19917354752983130, 7.196541539523007458 ) ) ;
#8154 = CARTESIAN_POINT ( 'NONE',  ( -4.745348413369673501, 58.35092235193497601, -12.64042052586673570 ) ) ;
#8155 =( BOUNDED_CURVE ( )  B_SPLINE_CURVE ( 2, ( #1620, #10827, #126, #5440, #12325, #15126, #14955, #10741, #12235, #16105, #3023, #2845, #8364 ),
 .UNSPECIFIED., .F., .F. ) 
 B_SPLINE_CURVE_WITH_KNOTS ( ( 3, 2, 2, 2, 2, 2, 3 ),
 ( 0.8194444444444444198, 0.8222222222222221877, 0.8277777777777777235, 0.8333333333333333703, 0.8388888888888889062, 0.8444444444444444420, 0.8472222222222222099 ),
 .UNSPECIFIED. ) 
 CURVE ( )  GEOMETRIC_REPRESENTATION_ITEM ( )  RATIONAL_B_SPLINE_CURVE ( ( 0.9755282581475768211, 0.9755282581475768211, 1.000000000000000000, 0.9510565162951535312, 1.000000000000000000, 0.9510565162951535312, 1.000000000000000000, 0.9510565162951535312, 1.000000000000000000, 0.9510565162951535312, 1.000000000000000000, 0.9755282581475768211, 0.9755282581475768211 ) ) 
 REPRESENTATION_ITEM ( '' )  );
#8156 = CARTESIAN_POINT ( 'NONE',  ( -3.556480217745532916E-14, 9.046025403784437202, -12.00000000000000000 ) ) ;
#8157 = CARTESIAN_POINT ( 'NONE',  ( 10.92172942406178926, 59.13000000000000256, 7.935100905948387684 ) ) ;
#8158 = CARTESIAN_POINT ( 'NONE',  ( 9.901291193213106467, 30.07383486385095495, 9.184156744704926822 ) ) ;
#8159 = LINE ( 'NONE', #13524, #10243 ) ;
#8160 = CARTESIAN_POINT ( 'NONE',  ( -5.372626086858939942, 49.37446523726847403, -12.39129945928973520 ) ) ;
#8161 = CARTESIAN_POINT ( 'NONE',  ( 11.50550600207001040, 63.69365567215912449, -7.062106151818590583 ) ) ;
#8162 = B_SPLINE_CURVE_WITH_KNOTS ( 'NONE', 3,
 ( #4610, #2021, #12826, #11327 ),
 .UNSPECIFIED., .F., .F.,
 ( 4, 4 ),
 ( 0.000000000000000000, 0.003336555488825435588 ),
 .UNSPECIFIED. ) ;
#8163 = CARTESIAN_POINT ( 'NONE',  ( 13.40526361136180356, 42.48724074931151051, -1.642292961744375335 ) ) ;
#8164 = CARTESIAN_POINT ( 'NONE',  ( -17.99988701463194474, 8.062211464643718628, -0.1761320247424245089 ) ) ;
#8165 = AXIS2_PLACEMENT_3D ( 'NONE', #5122, #6449, #861 ) ;
#8166 = VERTEX_POINT ( 'NONE', #5835 ) ;
#8167 = CARTESIAN_POINT ( 'NONE',  ( -3.320475467054404886E-07, 70.18000001193918536, -13.49999999999999467 ) ) ;
#8168 = CARTESIAN_POINT ( 'NONE',  ( 6.767892274421971166, 80.93000000000000682, 11.68099457074693603 ) ) ;
#8169 = CARTESIAN_POINT ( 'NONE',  ( 4.171729424061789260, 11.83000000000000718, 12.83926296998457239 ) ) ;
#8170 = ORIENTED_EDGE ( 'NONE', *, *, #6979, .T. ) ;
#8171 = CARTESIAN_POINT ( 'NONE',  ( -5.673269603926692994, 43.38613141203421719, -12.25006288933690968 ) ) ;
#8172 = CARTESIAN_POINT ( 'NONE',  ( -7.500000000000000000, 103.1860286984271795, 9.367496997597605457 ) ) ;
#8173 = CARTESIAN_POINT ( 'NONE',  ( 7.050225702995494892, 60.91835954970743927, -11.51657226464040029 ) ) ;
#8174 = CARTESIAN_POINT ( 'NONE',  ( 2.621994543952811015E-15, 8.179999999999994387, -14.19474002721660355 ) ) ;
#8175 = CARTESIAN_POINT ( 'NONE',  ( 2.104705901570253168, 71.75572894129780366, 13.33549315723480966 ) ) ;
#8176 = CARTESIAN_POINT ( 'NONE',  ( 12.44807024653844785, 57.62036106608136521, -5.224809667552474224 ) ) ;
#8177 = EDGE_CURVE ( 'NONE', #225, #7733, #13671, .T. ) ;
#8178 = CARTESIAN_POINT ( 'NONE',  ( -11.76794919243112325, 66.07999999999999829, 3.823638476888994386 ) ) ;
#8179 = CARTESIAN_POINT ( 'NONE',  ( -9.520470885617715595, 80.63000000000000966, -6.917026985038136289 ) ) ;
#8180 = ADVANCED_FACE ( 'NONE', ( #4587 ), #12626, .F. ) ;
#8181 = CARTESIAN_POINT ( 'NONE',  ( -11.01735871152694379, 47.22449060650489372, 7.813986986152833047 ) ) ;
#8182 = CIRCLE ( 'NONE', #13782, 26.00000000000000355 ) ;
#8183 = CARTESIAN_POINT ( 'NONE',  ( 1.771727720396010897, 46.11629509651881875, -13.49999888936976156 ) ) ;
#8184 = CARTESIAN_POINT ( 'NONE',  ( 0.6926531483078161022, 8.027905821154647015, -18.11545820097779469 ) ) ;
#8185 = CARTESIAN_POINT ( 'NONE',  ( 10.01122869418810524, -99.99999999999997158, 14.34650401988984747 ) ) ;
#8186 = CARTESIAN_POINT ( 'NONE',  ( -11.20634389893962712, 10.00000000000000178, -4.929649438907175885 ) ) ;
#8187 = CARTESIAN_POINT ( 'NONE',  ( -4.711679271994916540, -61.39687499999984510, 11.37499999999960210 ) ) ;
#8188 = DIRECTION ( 'NONE',  ( 0.000000000000000000, 0.000000000000000000, 1.000000000000000000 ) ) ;
#8189 = CARTESIAN_POINT ( 'NONE',  ( 12.43340273364695747, 33.62204941335177466, -5.272404384565503754 ) ) ;
#8190 = CARTESIAN_POINT ( 'NONE',  ( -5.043811212648944498, 73.36206509383546859, -12.52241046721988127 ) ) ;
#8191 = CARTESIAN_POINT ( 'NONE',  ( 7.500000000000000888, 102.9300000000000068, -9.367496997597600128 ) ) ;
#8192 = ORIENTED_EDGE ( 'NONE', *, *, #2992, .F. ) ;
#8193 = CARTESIAN_POINT ( 'NONE',  ( -3.489578404781044974, 62.55452843961951714, 13.04738054726565721 ) ) ;
#8194 = ORIENTED_EDGE ( 'NONE', *, *, #5923, .F. ) ;
#8195 = CARTESIAN_POINT ( 'NONE',  ( -9.520470885617717371, -13.76999999999999780, 6.917026985038133624 ) ) ;
#8196 = CARTESIAN_POINT ( 'NONE',  ( -8.043339635997652337, -67.60624999999984652, 8.043339635996300530 ) ) ;
#8197 = CARTESIAN_POINT ( 'NONE',  ( -12.16175685827595210, 44.14530326537092009, 5.861221165930757593 ) ) ;
#8198 = CARTESIAN_POINT ( 'NONE',  ( -7.499999999999996447, -23.75733333946868697, -9.035253535952438853 ) ) ;
#8199 = CARTESIAN_POINT ( 'NONE',  ( -13.49999999999999822, 47.07999999999999829, 4.386415899144235908 ) ) ;
#8200 = CARTESIAN_POINT ( 'NONE',  ( -13.45347138943250798, 70.96881323304897649, 1.119889726645023176 ) ) ;
#8201 = EDGE_CURVE ( 'NONE', #10469, #10491, #5578, .T. ) ;
#8202 = PRODUCT_DEFINITION_SHAPE ( 'NONE', 'NONE',  #3939 ) ;
#8203 = CARTESIAN_POINT ( 'NONE',  ( 18.62500000000064659, -60.39062499999985079, -7.714727599197336083 ) ) ;
#8204 = CARTESIAN_POINT ( 'NONE',  ( -13.47769472573310523, 67.89946296695690364, -0.8856965346868491684 ) ) ;
#8205 = CARTESIAN_POINT ( 'NONE',  ( -1.564113515457998572E-12, -79.08749999999980673, 18.62500000000000000 ) ) ;
#8206 = CARTESIAN_POINT ( 'NONE',  ( 13.05062916916600280, 54.30688700786019751, 3.454156714176291665 ) ) ;
#8207 = CARTESIAN_POINT ( 'NONE',  ( 0.000000000000000000, 80.93000000000000682, 0.000000000000000000 ) ) ;
#8208 = CARTESIAN_POINT ( 'NONE',  ( -11.82157965976159808, 64.68840243461779949, -6.519625715133806843 ) ) ;
#8209 = VERTEX_POINT ( 'NONE', #11044 ) ;
#8210 = CARTESIAN_POINT ( 'NONE',  ( -8.343458848123578520, 63.48000000000001108, -11.48378591275254124 ) ) ;
#8211 = CARTESIAN_POINT ( 'NONE',  ( -13.33969213930383013, 35.00272133652679685, 2.074452581059428091 ) ) ;
#8212 = ORIENTED_EDGE ( 'NONE', *, *, #422, .T. ) ;
#8213 = CARTESIAN_POINT ( 'NONE',  ( 13.43072676519339659, 78.38231396256115602, 1.366956873940078587 ) ) ;
#8214 = CARTESIAN_POINT ( 'NONE',  ( 0.6607497744049288801, -1.070778138966299504E-15, -12.02517454154194709 ) ) ;
#8215 = PRODUCT_DEFINITION_FORMATION_WITH_SPECIFIED_SOURCE ( 'ANY', '', #12276, .NOT_KNOWN. ) ;
#8216 = CARTESIAN_POINT ( 'NONE',  ( 7.500000000000000888, -23.02360215807748034, 9.261711852864909389 ) ) ;
#8217 = CARTESIAN_POINT ( 'NONE',  ( 8.548604269041621961, 72.85217239673389145, -10.44934178869447905 ) ) ;
#8218 = CARTESIAN_POINT ( 'NONE',  ( -3.636496289402156190, -13.46999999999999531, 11.19198476289190758 ) ) ;
#8219 = DIRECTION ( 'NONE',  ( 0.000000000000000000, 1.000000000000000000, 0.000000000000000000 ) ) ;
#8220 = CARTESIAN_POINT ( 'NONE',  ( -13.49999999999999822, -11.92000000000000348, 4.386415899144235908 ) ) ;
#8221 = CARTESIAN_POINT ( 'NONE',  ( -13.50000000000000000, 70.92999999999999261, -3.306546357697853733E-15 ) ) ;
#8222 = CARTESIAN_POINT ( 'NONE',  ( -13.47987952135760636, 52.90456830356593798, -0.7369079465333779888 ) ) ;
#8223 = ADVANCED_FACE ( 'NONE', ( #4410 ), #3069, .F. ) ;
#8224 = CARTESIAN_POINT ( 'NONE',  ( 9.520470885617717371, 49.72999999999999687, -6.917026985038131848 ) ) ;
#8225 = CARTESIAN_POINT ( 'NONE',  ( -4.171729424061787483, 63.32999999999999829, -12.83926296998457417 ) ) ;
#8226 = CARTESIAN_POINT ( 'NONE',  ( 12.49292108473675356, 51.24384918054708038, 5.116345218930953287 ) ) ;
#8227 = CARTESIAN_POINT ( 'NONE',  ( -5.505992092405349148, 37.37965637996170898, -12.32618761653607820 ) ) ;
#8228 = CARTESIAN_POINT ( 'NONE',  ( 11.19183201792044535, 36.14618292256778886, 7.549567337428954694 ) ) ;
#8229 = CARTESIAN_POINT ( 'NONE',  ( -8.043339635996300530, -96.74374999999980673, -8.043339635997652337 ) ) ;
#8230 = CARTESIAN_POINT ( 'NONE',  ( -10.88893267353162209, 74.23195708089093614, 7.985199624914343985 ) ) ;
#8231 = CARTESIAN_POINT ( 'NONE',  ( -13.15105693501601003, 77.03838810807653203, 3.057644733085780331 ) ) ;
#8232 = CARTESIAN_POINT ( 'NONE',  ( -10.15331777804710356, 79.58698102410616571, -8.908116406432318612 ) ) ;
#8233 = DIRECTION ( 'NONE',  ( 0.000000000000000000, 0.000000000000000000, 1.000000000000000000 ) ) ;
#8234 = CARTESIAN_POINT ( 'NONE',  ( 3.114363690246614080, 80.93000000000004945, 12.90281209101391369 ) ) ;
#8235 = CARTESIAN_POINT ( 'NONE',  ( -8.343458848123578520, 7.480000000000002203, -11.48378591275254124 ) ) ;
#8236 = CARTESIAN_POINT ( 'NONE',  ( 2.279995255611139653E-15, 6.179999999999999716, -12.37355403259654985 ) ) ;
#8237 = CARTESIAN_POINT ( 'NONE',  ( -11.76794919243112325, 47.92999999999999972, -2.882316262207890869E-15 ) ) ;
#8238 = CARTESIAN_POINT ( 'NONE',  ( -7.714727599197335195, -21.85312499999995239, -18.62500000000064304 ) ) ;
#8239 = CARTESIAN_POINT ( 'NONE',  ( -4.171729424061791036, -6.469999999999996199, 12.83926296998457239 ) ) ;
#8240 = CARTESIAN_POINT ( 'NONE',  ( -12.99798557104473495, 40.79969145139732234, -3.647469504750259883 ) ) ;
#8241 = CARTESIAN_POINT ( 'NONE',  ( 4.171729424061791924, 36.03000000000000114, -12.83926296998457239 ) ) ;
#8242 = CARTESIAN_POINT ( 'NONE',  ( 13.11911623483412725, 75.54314320642072289, -3.184815548587396794 ) ) ;
#8243 = DIRECTION ( 'NONE',  ( -0.000000000000000000, -1.000000000000000000, -0.000000000000000000 ) ) ;
#8244 = CARTESIAN_POINT ( 'NONE',  ( 11.76794919243112325, 34.28000000000000114, 3.823638476888996607 ) ) ;
#8245 = CARTESIAN_POINT ( 'NONE',  ( -5.892354067706281562, 58.39472778308726220, -12.14630281014331281 ) ) ;
#8246 = CARTESIAN_POINT ( 'NONE',  ( -10.92957602604999146, 9.999999999999998224, 4.954227274842499362 ) ) ;
#8247 = CARTESIAN_POINT ( 'NONE',  ( -4.023268246324633536E-14, 60.18000000000000682, -13.50000000000000000 ) ) ;
#8248 = CARTESIAN_POINT ( 'NONE',  ( 9.135248883881359916, 30.03565898711111259, 9.940076883576240974 ) ) ;
#8249 = CARTESIAN_POINT ( 'NONE',  ( -13.50000000000000000, 57.92999999999999972, -3.306546357697853733E-15 ) ) ;
#8250 = CARTESIAN_POINT ( 'NONE',  ( -10.03685761320076075, 49.58118651522960363, -9.028742826659037490 ) ) ;
#8251 = CIRCLE ( 'NONE', #13313, 26.00000000000000355 ) ;
#8252 = CARTESIAN_POINT ( 'NONE',  ( 12.88414385799500117, 63.28531013651519999, 4.031028846843240920 ) ) ;
#8253 = CARTESIAN_POINT ( 'NONE',  ( 12.36777513855581390, 42.23235083080415109, 5.411869368907026967 ) ) ;
#8254 = CARTESIAN_POINT ( 'NONE',  ( -18.71385749420392841, 7.854010659623983592, 1.541332980592373225 ) ) ;
#8255 = ADVANCED_FACE ( 'NONE', ( #8029 ), #12167, .F. ) ;
#8256 = ORIENTED_EDGE ( 'NONE', *, *, #14132, .T. ) ;
#8257 = CARTESIAN_POINT ( 'NONE',  ( -7.416407864998736166, 3.346025403784435248, -10.20780970022448031 ) ) ;
#8258 = LINE ( 'NONE', #9672, #11854 ) ;
#8259 = CARTESIAN_POINT ( 'NONE',  ( -13.50000000000000000, 10.92999999999999616, -3.469446951953614189E-15 ) ) ;
#8260 = ORIENTED_EDGE ( 'NONE', *, *, #2675, .T. ) ;
#8261 = CARTESIAN_POINT ( 'NONE',  ( -3.110033635544421582, 43.29182205780823267, -13.14495504916145485 ) ) ;
#8262 = CARTESIAN_POINT ( 'NONE',  ( -7.500000000000000000, 108.3824470675415341, -4.067225351102824682 ) ) ;
#8263 = CARTESIAN_POINT ( 'NONE',  ( 11.56001456171610720, 60.68998491048684940, -6.972525382906384905 ) ) ;
#8264 = CARTESIAN_POINT ( 'NONE',  ( 4.171729424061789260, 9.830000000000005400, 12.83926296998457239 ) ) ;
#8265 = CARTESIAN_POINT ( 'NONE',  ( -13.16986379959834252, -22.89374999999994387, -13.16986379960055054 ) ) ;
#8266 = CARTESIAN_POINT ( 'NONE',  ( 13.31917153282089039, 66.50765729681475591, -2.211295458653834256 ) ) ;
#8267 = CARTESIAN_POINT ( 'NONE',  ( 3.121749870751446387, 56.79230302867953384, 13.13415442199402960 ) ) ;
#8268 = CARTESIAN_POINT ( 'NONE',  ( 7.272992578804311492, 55.87999999999998835, -10.01041549318726709 ) ) ;
#8269 = CARTESIAN_POINT ( 'NONE',  ( -11.76794919243112325, 71.92999999999999261, -2.882316262207890869E-15 ) ) ;
#8270 = AXIS2_PLACEMENT_3D ( 'NONE', #867, #4946, #16781 ) ;
#8271 = CARTESIAN_POINT ( 'NONE',  ( -11.68579365184739061, 47.18153587550196448, 6.763020047883973263 ) ) ;
#8272 = DIRECTION ( 'NONE',  ( 1.000000000000000000, 0.000000000000000000, 8.379555213223520053E-14 ) ) ;
#8273 = CARTESIAN_POINT ( 'NONE',  ( 11.51355534411690762, -100.0000000000000284, 13.49408347815985465 ) ) ;
#8274 = CARTESIAN_POINT ( 'NONE',  ( -6.594413527910950812, 56.43719554618320444, 11.79074946145723146 ) ) ;
#8275 = CARTESIAN_POINT ( 'NONE',  ( 11.37499999999999645, -7.250000000000000000, 9.531744055041752924E-13 ) ) ;
#8276 = CARTESIAN_POINT ( 'NONE',  ( -10.92172942406179104, 52.22999999999999687, 7.935100905948387684 ) ) ;
#8277 = CARTESIAN_POINT ( 'NONE',  ( 13.04518082719695649, 33.55387728658139679, -3.474737096573298878 ) ) ;
#8278 = CARTESIAN_POINT ( 'NONE',  ( -10.11735578038046235, 9.999999999999994671, 6.713151495386600942 ) ) ;
#8279 = CARTESIAN_POINT ( 'NONE',  ( -8.247312284513380831, 7.985359057032879626, -16.32246862014511990 ) ) ;
#8280 = CARTESIAN_POINT ( 'NONE',  ( -11.76794919243112325, 25.08000000000001251, 3.823638476888994386 ) ) ;
#8281 = EDGE_CURVE ( 'NONE', #2565, #15915, #2776, .T. ) ;
#8282 = ORIENTED_EDGE ( 'NONE', *, *, #14268, .F. ) ;
#8283 = CARTESIAN_POINT ( 'NONE',  ( -13.49999999999999822, 43.07999999999999829, 4.386415899144235020 ) ) ;
#8284 = VERTEX_POINT ( 'NONE', #6616 ) ;
#8285 = AXIS2_PLACEMENT_3D ( 'NONE', #4681, #11401, #11226 ) ;
#8286 = CARTESIAN_POINT ( 'NONE',  ( -13.46460078802627258, 40.89617066210697516, -0.9799208027847087221 ) ) ;
#8287 = CARTESIAN_POINT ( 'NONE',  ( -18.62500000000064659, -49.91562499999989910, 7.714727599197333419 ) ) ;
#8288 = CARTESIAN_POINT ( 'NONE',  ( -13.47942042829293641, 43.95571666567489189, 0.7453506697733148778 ) ) ;
#8289 = CARTESIAN_POINT ( 'NONE',  ( -8.845307762532344853, 8.062143948122718839, 15.67790026899615619 ) ) ;
#8290 = CARTESIAN_POINT ( 'NONE',  ( 4.171729424061791924, 43.03000000000000114, -12.83926296998457239 ) ) ;
#8291 = CARTESIAN_POINT ( 'NONE',  ( -13.44824536596492237, 70.97096667731948116, 1.181153100867837313 ) ) ;
#8292 = VECTOR ( 'NONE', #10412, 1000.000000000000000 ) ;
#8293 = CARTESIAN_POINT ( 'NONE',  ( -18.62500000000000000, -17.72499999999994102, -1.562973063126292757E-12 ) ) ;
#8294 = CARTESIAN_POINT ( 'NONE',  ( -6.505070197219007255, 67.41913341053678721, -11.83553212610193128 ) ) ;
#8295 = CARTESIAN_POINT ( 'NONE',  ( 7.714727599197340524, -39.57812499999989342, 18.62500000000063949 ) ) ;
#8296 = CARTESIAN_POINT ( 'NONE',  ( 12.92435448664457631, 54.56979870081450912, -3.901149989671772289 ) ) ;
#8297 = CARTESIAN_POINT ( 'NONE',  ( -1.103415079611737237, 64.21967456855061585, -13.45889604906427195 ) ) ;
#8298 = ADVANCED_FACE ( 'NONE', ( #2777 ), #14796, .T. ) ;
#8299 = EDGE_LOOP ( 'NONE', ( #8458, #13259, #10389, #7622 ) ) ;
#8300 = DIRECTION ( 'NONE',  ( -0.000000000000000000, 1.000000000000000000, -0.000000000000000000 ) ) ;
#8301 = CARTESIAN_POINT ( 'NONE',  ( -13.27056125883154714, 34.84229683454460513, -2.490662099278118546 ) ) ;
#8302 = VERTEX_POINT ( 'NONE', #2688 ) ;
#8303 = CARTESIAN_POINT ( 'NONE',  ( 12.47629078338616537, 78.24213358348909253, 5.161934717677671536 ) ) ;
#8304 = CARTESIAN_POINT ( 'NONE',  ( -11.82076925184314931, -1.497824325258514019E-15, -5.475814512136048862 ) ) ;
#8305 = DIRECTION ( 'NONE',  ( 0.000000000000000000, 1.000000000000000000, 0.000000000000000000 ) ) ;
#8306 = CARTESIAN_POINT ( 'NONE',  ( 7.500000000000001776, -23.02061778433118278, -9.262340467025641289 ) ) ;
#8307 = CARTESIAN_POINT ( 'NONE',  ( 10.33443572568632085, 72.76295794329135447, -8.686189713967003456 ) ) ;
#8308 = CARTESIAN_POINT ( 'NONE',  ( 18.99999999999999289, 7.773118517290098062, 1.732050807568941586 ) ) ;
#8309 = CARTESIAN_POINT ( 'NONE',  ( 13.50000000000000355, -13.42000000000000703, -4.386415899144233244 ) ) ;
#8310 = CARTESIAN_POINT ( 'NONE',  ( -13.49999999999999822, 76.77999999999998693, -4.386415899144240349 ) ) ;
#8311 = CARTESIAN_POINT ( 'NONE',  ( -11.31104933256506762, 52.65366644603506074, -7.369657635140959506 ) ) ;
#8312 = CARTESIAN_POINT ( 'NONE',  ( 7.272992578804311492, 43.87999999999999545, -10.01041549318726709 ) ) ;
#8313 = CARTESIAN_POINT ( 'NONE',  ( 8.343458848123583849, 62.88000000000000256, -11.48378591275253768 ) ) ;
#8314 = DIRECTION ( 'NONE',  ( 0.000000000000000000, 0.000000000000000000, 1.000000000000000000 ) ) ;
#8315 = CARTESIAN_POINT ( 'NONE',  ( 11.67243386019293716, 69.17774755439334911, 6.782755736582077866 ) ) ;
#8316 = LINE ( 'NONE', #7240, #5635 ) ;
#8317 = CARTESIAN_POINT ( 'NONE',  ( 1.708800344670653191E-06, 35.68004753840243382, 13.49999999999978328 ) ) ;
#8318 = CARTESIAN_POINT ( 'NONE',  ( -4.711679271994915652, -101.9468749999997783, 11.37499999999960210 ) ) ;
#8319 = CARTESIAN_POINT ( 'NONE',  ( -10.48937736199612480, 74.25448204741239522, 8.498420214693403807 ) ) ;
#8320 = CARTESIAN_POINT ( 'NONE',  ( -13.49504752740739555, 76.94266908463271193, 0.3689546535713391640 ) ) ;
#8321 = ADVANCED_FACE ( 'NONE', ( #8119 ), #13485, .T. ) ;
#8322 = CARTESIAN_POINT ( 'NONE',  ( -4.310646433793312582, 79.33501006869653338, -12.79332600423342470 ) ) ;
#8323 = CARTESIAN_POINT ( 'NONE',  ( -12.00000000000000178, 0.7960254037844517461, -2.718289652585035561E-15 ) ) ;
#8324 = CARTESIAN_POINT ( 'NONE',  ( 2.138189846611488143, 3.756881418804832506, 13.50000003176731589 ) ) ;
#8325 = CARTESIAN_POINT ( 'NONE',  ( -9.520470885617715595, -8.369999999999995666, -6.917026985038136289 ) ) ;
#8326 = CARTESIAN_POINT ( 'NONE',  ( 3.636496289402154414, 45.82999999999999829, 11.19198476289190936 ) ) ;
#8327 = CARTESIAN_POINT ( 'NONE',  ( -8.891200544363830713E-16, 2.680000000000005045, 13.49999999999999822 ) ) ;
#8328 = FACE_OUTER_BOUND ( 'NONE', #12482, .T. ) ;
#8329 = CARTESIAN_POINT ( 'NONE',  ( 13.49033203594054697, 75.44763660926943771, -0.5127258900949339671 ) ) ;
#8330 = CARTESIAN_POINT ( 'NONE',  ( 18.62500000000007105, 1.797534614761401329E-30, -0.8911350689967181271 ) ) ;
#8331 = CARTESIAN_POINT ( 'NONE',  ( -12.21084993027352716, 41.14197536515471398, 5.780306110364526795 ) ) ;
#8332 = AXIS2_PLACEMENT_3D ( 'NONE', #5653, #12177, #68 ) ;
#8333 = CARTESIAN_POINT ( 'NONE',  ( 0.000000000000000000, 80.93000000000000682, -13.50000000000000000 ) ) ;
#8334 = CARTESIAN_POINT ( 'NONE',  ( 6.229800185101045606, 44.90808656577910085, 11.97664669193207132 ) ) ;
#8335 = CARTESIAN_POINT ( 'NONE',  ( -13.49999999999999822, 54.77999999999998693, -4.386415899144240349 ) ) ;
#8336 = DIRECTION ( 'NONE',  ( 0.000000000000000000, 0.000000000000000000, -1.000000000000000000 ) ) ;
#8337 = DIRECTION ( 'NONE',  ( -1.000000000000000000, -1.772429021826857464E-16, 0.000000000000000000 ) ) ;
#8338 = CARTESIAN_POINT ( 'NONE',  ( -7.304906251596263722, 49.45255025094410684, -11.35316560862786339 ) ) ;
#8339 = CARTESIAN_POINT ( 'NONE',  ( 10.90660565521129044, 63.12913462907602025, 7.957536297550788618 ) ) ;
#8340 = CARTESIAN_POINT ( 'NONE',  ( 13.48614902602365362, 42.45108007468103040, -0.6119829615113150378 ) ) ;
#8341 = CARTESIAN_POINT ( 'NONE',  ( 3.563393355819833186, 38.80806997300490480, 13.02747425359752675 ) ) ;
#8342 = ORIENTED_EDGE ( 'NONE', *, *, #5396, .F. ) ;
#8343 = CARTESIAN_POINT ( 'NONE',  ( -7.576616670048093940E-16, 75.67999999999997840, 12.37355403259654807 ) ) ;
#8344 = CARTESIAN_POINT ( 'NONE',  ( 12.50000000000000000, -18.00000000000000355, 8.999999999999998224 ) ) ;
#8345 = CARTESIAN_POINT ( 'NONE',  ( 4.711679271994910323, -19.77187499999995168, -11.37499999999960387 ) ) ;
#8346 = CARTESIAN_POINT ( 'NONE',  ( -8.549982208541774191E-16, 8.679999999999994387, 14.19474002721660355 ) ) ;
#8347 = ORIENTED_EDGE ( 'NONE', *, *, #17236, .F. ) ;
#8348 = CARTESIAN_POINT ( 'NONE',  ( -4.129969626718125397, 43.32850618201838699, -12.85291258290743954 ) ) ;
#8349 = CARTESIAN_POINT ( 'NONE',  ( 0.000000000000000000, 80.93000000000000682, 0.000000000000000000 ) ) ;
#8350 = CARTESIAN_POINT ( 'NONE',  ( 12.91929742426344419, 60.57042407115622495, -3.917859330391978645 ) ) ;
#8351 = CARTESIAN_POINT ( 'NONE',  ( 10.92172942406178926, 7.129999999999997229, 7.935100905948385908 ) ) ;
#8352 = LINE ( 'NONE', #378, #4008 ) ;
#8353 = CARTESIAN_POINT ( 'NONE',  ( 13.44750236278916589, 66.38875313069046058, 1.189447314180342330 ) ) ;
#8354 = CARTESIAN_POINT ( 'NONE',  ( 8.142818167418832687, 56.98927294900627771, 10.76880729706688200 ) ) ;
#8355 = CARTESIAN_POINT ( 'NONE',  ( 11.76794919243112325, 55.42999999999999972, 1.441158131103945434E-15 ) ) ;
#8356 = CARTESIAN_POINT ( 'NONE',  ( 9.520470885617715595, 70.12999999999999545, 6.917026985038134512 ) ) ;
#8357 = CARTESIAN_POINT ( 'NONE',  ( -11.59131112589550838, 47.18803745467646138, 6.922104400456148277 ) ) ;
#8358 = ADVANCED_FACE ( 'NONE', ( #13569 ), #10844, .T. ) ;
#8359 = CARTESIAN_POINT ( 'NONE',  ( 5.515696437122907803, 45.97993358946585118, -12.32182730336969634 ) ) ;
#8360 = CARTESIAN_POINT ( 'NONE',  ( 1.102182119232618108E-15, 108.9300000000000068, -6.000000000000001776 ) ) ;
#8361 = CARTESIAN_POINT ( 'NONE',  ( 8.632143809700615122, 30.84828256068346164, -10.38016917814384144 ) ) ;
#8362 = CARTESIAN_POINT ( 'NONE',  ( -7.689041659587561917, 9.999999999999992895, -10.05412496806502887 ) ) ;
#8363 = CARTESIAN_POINT ( 'NONE',  ( -4.711679271993004292, -55.15312499999986784, -11.37500000000039435 ) ) ;
#8364 = CARTESIAN_POINT ( 'NONE',  ( 2.445080149700053643E-15, 39.17999999999999972, -13.50000000000000000 ) ) ;
#8365 = CARTESIAN_POINT ( 'NONE',  ( 11.33052969111197150, 33.70514019894347513, -7.339663749698858375 ) ) ;
#8366 = LINE ( 'NONE', #4195, #12779 ) ;
#8367 = CARTESIAN_POINT ( 'NONE',  ( 0.6587682488342593290, 40.15634701798867212, -13.48451925025889864 ) ) ;
#8368 = CARTESIAN_POINT ( 'NONE',  ( -7.272992578804307939, 24.48000000000000398, -10.01041549318726886 ) ) ;
#8369 = ORIENTED_EDGE ( 'NONE', *, *, #3366, .T. ) ;
#8370 = CARTESIAN_POINT ( 'NONE',  ( -3.942068916870681949, 62.53825775923972685, 12.91162929084544331 ) ) ;
#8371 = AXIS2_PLACEMENT_3D ( 'NONE', #13762, #4238, #8233 ) ;
#8372 = VERTEX_POINT ( 'NONE', #17378 ) ;
#8373 = CARTESIAN_POINT ( 'NONE',  ( 9.520470885617717371, -15.26999999999999957, -6.917026985038131848 ) ) ;
#8374 = CARTESIAN_POINT ( 'NONE',  ( -18.62500000000064659, -66.56562499999988347, 7.714727599197333419 ) ) ;
#8375 = CARTESIAN_POINT ( 'NONE',  ( -13.45911978172200030, 43.89364414836797579, -1.050976612551407952 ) ) ;
#8376 = CARTESIAN_POINT ( 'NONE',  ( -8.177092975168962496, 7.956016782093530360, 16.47957145870427453 ) ) ;
#8377 = CARTESIAN_POINT ( 'NONE',  ( 13.50000000000000355, 30.57999999999999829, -4.386415899144233244 ) ) ;
#8378 = CARTESIAN_POINT ( 'NONE',  ( -8.343458848123582072, 49.37999999999998835, 11.48378591275254124 ) ) ;
#8379 = VECTOR ( 'NONE', #969, 1000.000000000000000 ) ;
#8380 = CARTESIAN_POINT ( 'NONE',  ( -18.62500000000000000, -51.02499999999986358, -1.562973063126292757E-12 ) ) ;
#8381 = CARTESIAN_POINT ( 'NONE',  ( -9.946115144241847617, 67.57636767219140950, -9.129800658857289974 ) ) ;
#8382 = CARTESIAN_POINT ( 'NONE',  ( -1.564113515457998370E-12, -88.48749999999975557, 18.62500000000000000 ) ) ;
#8383 = CARTESIAN_POINT ( 'NONE',  ( 10.93217480255018792, 54.72939847821437098, -7.926001620418541727 ) ) ;
#8384 = CARTESIAN_POINT ( 'NONE',  ( -3.235480449190796914, 64.29635529473749500, -13.10656066990217994 ) ) ;
#8385 = ORIENTED_EDGE ( 'NONE', *, *, #15485, .F. ) ;
#8386 = CARTESIAN_POINT ( 'NONE',  ( -2.138189944381240881, 64.60311857767972299, 13.49999999999999822 ) ) ;
#8387 = CARTESIAN_POINT ( 'NONE',  ( -11.84697983171742308, 34.69028098126747750, -6.472949912695511898 ) ) ;
#8388 = PRODUCT_DEFINITION ( 'UNKNOWN', '', #16376, #13374 ) ;
#8389 = ORIENTED_EDGE ( 'NONE', *, *, #3103, .T. ) ;
#8390 = CARTESIAN_POINT ( 'NONE',  ( 12.02766759040286537, 78.20374727343299526, 6.138006497614846069 ) ) ;
#8391 = DIRECTION ( 'NONE',  ( 0.000000000000000000, -1.000000000000000000, 0.000000000000000000 ) ) ;
#8392 = CARTESIAN_POINT ( 'NONE',  ( 7.500000000000004441, -25.82389322351430039, -7.532295102519075414 ) ) ;
#8393 = CARTESIAN_POINT ( 'NONE',  ( 11.30732042667622217, 72.70668772296686200, -7.376702573910818295 ) ) ;
#8394 = CARTESIAN_POINT ( 'NONE',  ( 12.10710496143796000, 78.64972431541795572, -5.972800933619774710 ) ) ;
#8395 = CARTESIAN_POINT ( 'NONE',  ( -8.343458848123576743, -18.52000000000000668, -11.48378591275254301 ) ) ;
#8396 = CARTESIAN_POINT ( 'NONE',  ( -8.343458848123576743, 64.47999999999998977, -11.48378591275254301 ) ) ;
#8397 = CARTESIAN_POINT ( 'NONE',  ( -13.46262499177027649, 52.89525612230203677, -1.006202793444178178 ) ) ;
#8398 = CARTESIAN_POINT ( 'NONE',  ( 9.520470885617715595, 43.13000000000000256, 6.917026985038134512 ) ) ;
#8399 = CARTESIAN_POINT ( 'NONE',  ( 3.636496289402157078, -17.96999999999999886, -11.19198476289190936 ) ) ;
#8400 = CARTESIAN_POINT ( 'NONE',  ( 10.92172942406178926, 59.13000000000000256, 7.935100905948387684 ) ) ;
#8401 = EDGE_CURVE ( 'NONE', #760, #10228, #16918, .T. ) ;
#8402 = CARTESIAN_POINT ( 'NONE',  ( -16.64312382832864046, 7.924527542031521321, -8.110285629053153755 ) ) ;
#8403 = CARTESIAN_POINT ( 'NONE',  ( 9.962334412389218130, 69.07724864637550866, 9.110570040184843066 ) ) ;
#8404 = CARTESIAN_POINT ( 'NONE',  ( -1.094976389599479960, 37.21933971898220506, -13.45805156410629166 ) ) ;
#8405 = CARTESIAN_POINT ( 'NONE',  ( -13.50000000000000000, 72.92999999999999261, -3.306546357697853733E-15 ) ) ;
#8406 = CARTESIAN_POINT ( 'NONE',  ( 1.561832610794586740E-12, -61.36249999999986215, -18.62500000000000000 ) ) ;
#8407 = CARTESIAN_POINT ( 'NONE',  ( -8.233788210363634619, 74.36659837790818983, 10.69896094284675847 ) ) ;
#8408 = CARTESIAN_POINT ( 'NONE',  ( -7.578294665328167312, 76.46427856810599621, -11.17381362175432358 ) ) ;
#8409 = CARTESIAN_POINT ( 'NONE',  ( 22.26874168100111362, 6.548282979925672542, 8.000000000000099476 ) ) ;
#8410 = DIRECTION ( 'NONE',  ( -0.4999999999999881761, 0.000000000000000000, -0.8660254037844454800 ) ) ;
#8411 = FACE_OUTER_BOUND ( 'NONE', #11186, .T. ) ;
#8412 = CARTESIAN_POINT ( 'NONE',  ( 8.343458848123578520, 30.98000000000000043, 11.48378591275254124 ) ) ;
#8413 = CARTESIAN_POINT ( 'NONE',  ( 7.272992578804311492, -3.120000000000004992, -10.01041549318726709 ) ) ;
#8414 = CARTESIAN_POINT ( 'NONE',  ( 9.520470885617715595, 43.13000000000000256, 6.917026985038134512 ) ) ;
#8415 = CARTESIAN_POINT ( 'NONE',  ( -2.138189944381236884, 1.256881422320270003, -13.50000000000000000 ) ) ;
#8416 = CARTESIAN_POINT ( 'NONE',  ( -2.816865131317705995, 32.57878533943133448, 13.20872976553534173 ) ) ;
#8417 = CARTESIAN_POINT ( 'NONE',  ( 13.24501161275586902, 75.52252332348925279, -2.622349305493431704 ) ) ;
#8418 = CARTESIAN_POINT ( 'NONE',  ( 10.05114101558813289, -5.362028352459332625E-15, -14.43934216884202293 ) ) ;
#8419 = CARTESIAN_POINT ( 'NONE',  ( -6.990220506518823207, 41.42075001818317048, 11.54933267199740499 ) ) ;
#8420 = EDGE_CURVE ( 'NONE', #15651, #42, #10984, .T. ) ;
#8421 = CARTESIAN_POINT ( 'NONE',  ( 1.146149308888379847, 52.13878882479240673, -13.45154095393029792 ) ) ;
#8422 = CARTESIAN_POINT ( 'NONE',  ( -0.8900169510020742303, 38.64814324494936670, 13.47797843473638046 ) ) ;
#8423 = CARTESIAN_POINT ( 'NONE',  ( 0.000000000000000000, 108.9300000000000068, 0.000000000000000000 ) ) ;
#8424 = CARTESIAN_POINT ( 'NONE',  ( -0.4935672077447687545, 55.19774674342932030, -13.49105727626698403 ) ) ;
#8425 = CARTESIAN_POINT ( 'NONE',  ( -3.349185717234338444, 49.30034724615263997, -13.08421705775778321 ) ) ;
#8426 = CARTESIAN_POINT ( 'NONE',  ( 8.447120960974235260, 63.00251278634441832, 10.55471404757047260 ) ) ;
#8427 = CARTESIAN_POINT ( 'NONE',  ( 13.48201631440997161, 42.45403165440193050, -0.6969096715845409795 ) ) ;
#8428 = CARTESIAN_POINT ( 'NONE',  ( 5.872522573940052837, 48.96601633533685316, -12.15592568072844948 ) ) ;
#8429 = CARTESIAN_POINT ( 'NONE',  ( -7.272992578804310604, 25.38000000000000256, 10.01041549318726709 ) ) ;
#8430 = ORIENTED_EDGE ( 'NONE', *, *, #1972, .F. ) ;
#8431 = CARTESIAN_POINT ( 'NONE',  ( -7.272992578804307939, 80.47999999999998977, -10.01041549318727064 ) ) ;
#8432 = CARTESIAN_POINT ( 'NONE',  ( -2.595053155729497796, 70.27330850474520219, -13.24824729708691251 ) ) ;
#8433 = CARTESIAN_POINT ( 'NONE',  ( -4.711679271994915652, -61.39687499999985221, 11.37499999999960210 ) ) ;
#8434 = CARTESIAN_POINT ( 'NONE',  ( 10.92172942406178926, 6.129999999999996341, 7.935100905948385908 ) ) ;
#8435 = ORIENTED_EDGE ( 'NONE', *, *, #3081, .F. ) ;
#8436 = CARTESIAN_POINT ( 'NONE',  ( -8.739346652766617041, 43.51675563888475295, -10.28954507209749814 ) ) ;
#8437 = CARTESIAN_POINT ( 'NONE',  ( -7.500000000000000000, 107.9394166107543214, -5.548846425319426068 ) ) ;
#8438 = CARTESIAN_POINT ( 'NONE',  ( 13.06095779972256388, 60.55178070539100332, -3.418504200385884761 ) ) ;
#8439 = CARTESIAN_POINT ( 'NONE',  ( -13.49999999999999822, 3.080000000000009841, 4.386415899144235908 ) ) ;
#8440 = CARTESIAN_POINT ( 'NONE',  ( 17.42428528562858148, 0.000000000000000000, -19.29752010712846300 ) ) ;
#8441 = CARTESIAN_POINT ( 'NONE',  ( 3.575946890483998608, 65.80826063327815234, 13.01961353005121325 ) ) ;
#8442 = CARTESIAN_POINT ( 'NONE',  ( 5.688864601221035322, 56.88665272175017407, 12.25002412551037345 ) ) ;
#8443 = CARTESIAN_POINT ( 'NONE',  ( -7.576616670048093940E-16, 63.67999999999997840, 12.37355403259654985 ) ) ;
#8444 = CARTESIAN_POINT ( 'NONE',  ( 13.50000000000000355, 35.58000000000000540, -4.386415899144233244 ) ) ;
#8445 = CARTESIAN_POINT ( 'NONE',  ( -11.76794919243112325, 62.78000000000000114, -3.823638476888998827 ) ) ;
#8446 = ADVANCED_FACE ( 'NONE', ( #12945 ), #5091, .F. ) ;
#8447 = CARTESIAN_POINT ( 'NONE',  ( -13.50089624978355651, 46.93407419958843008, 0.1205557709537223021 ) ) ;
#8448 = CARTESIAN_POINT ( 'NONE',  ( 11.21015142536170472, 45.71264101303631122, -7.528624130298565476 ) ) ;
#8449 = CARTESIAN_POINT ( 'NONE',  ( 0.000000000000000000, 80.93000000000000682, 0.000000000000000000 ) ) ;
#8450 = CARTESIAN_POINT ( 'NONE',  ( 0.3535656791965426926, 8.055112074840369729, 18.02368563757056563 ) ) ;
#8451 = CARTESIAN_POINT ( 'NONE',  ( 5.712863636558116909, 30.97219126872883166, -12.23179765126074159 ) ) ;
#8452 = CARTESIAN_POINT ( 'NONE',  ( -0.4447041180500230784, 56.66422576703538283, 13.50000000034898129 ) ) ;
#8453 = CARTESIAN_POINT ( 'NONE',  ( 8.043339635996300530, -97.81874999999976694, 8.043339635997654113 ) ) ;
#8454 = CARTESIAN_POINT ( 'NONE',  ( 12.63326194426385740, 33.25766702093661564, 4.760573950502951845 ) ) ;
#8455 = CARTESIAN_POINT ( 'NONE',  ( -15.28534784291377235, 6.548267719634618622, -18.06260399879766965 ) ) ;
#8456 = CARTESIAN_POINT ( 'NONE',  ( 4.747830034773906860, 40.00896622368698274, -12.63869487930051250 ) ) ;
#8457 = CARTESIAN_POINT ( 'NONE',  ( -11.76794919243112325, 22.08000000000000540, 3.823638476888994386 ) ) ;
#8458 = ORIENTED_EDGE ( 'NONE', *, *, #16476, .T. ) ;
#8459 = CARTESIAN_POINT ( 'NONE',  ( -11.54364396704453455, 62.19215880004057340, 7.031275361532858703 ) ) ;
#8460 = VERTEX_POINT ( 'NONE', #11627 ) ;
#8461 = AXIS2_PLACEMENT_3D ( 'NONE', #155, #8305, #6975 ) ;
#8462 = CARTESIAN_POINT ( 'NONE',  ( -11.76794919243112325, -17.06999999999999318, -2.602085213965210642E-15 ) ) ;
#8463 = CARTESIAN_POINT ( 'NONE',  ( -1.564113515457998370E-12, -69.68749999999984368, 18.62500000000000000 ) ) ;
#8464 = CARTESIAN_POINT ( 'NONE',  ( -12.30465744001379491, 44.13348343788968009, 5.561576354214327722 ) ) ;
#8465 = CARTESIAN_POINT ( 'NONE',  ( -7.999999999999776179, 7.773118517290098062, -17.32050807568887762 ) ) ;
#8466 = AXIS2_PLACEMENT_3D ( 'NONE', #3313, #8727, #11278 ) ;
#8467 = CARTESIAN_POINT ( 'NONE',  ( 10.92172942406179104, 33.72999999999999687, -7.935100905948385908 ) ) ;
#8468 = CARTESIAN_POINT ( 'NONE',  ( 4.171729424061789260, 49.82999999999999829, 12.83926296998457417 ) ) ;
#8469 = CARTESIAN_POINT ( 'NONE',  ( -4.051944394872408317, 46.32562282393774922, -12.87823981119249162 ) ) ;
#8470 = CARTESIAN_POINT ( 'NONE',  ( -7.810976174431880636, 67.47450371884892206, -11.01108770444237805 ) ) ;
#8471 = CARTESIAN_POINT ( 'NONE',  ( 18.62499999999935341, -74.95937499999980957, 7.714727599200469577 ) ) ;
#8472 = CARTESIAN_POINT ( 'NONE',  ( 10.67668064206492673, 54.11596557450559430, 8.261870253898289107 ) ) ;
#8473 = VECTOR ( 'NONE', #1054, 1000.000000000000000 ) ;
#8474 = CARTESIAN_POINT ( 'NONE',  ( -4.764317252036915917, 64.35142252853242439, -12.63898182757053590 ) ) ;
#8475 = ORIENTED_EDGE ( 'NONE', *, *, #3286, .T. ) ;
#8476 = CARTESIAN_POINT ( 'NONE',  ( -10.29247617992475305, 34.59463260972069776, -8.736624418168057460 ) ) ;
#8477 = CARTESIAN_POINT ( 'NONE',  ( -9.552639591052204498E-13, -45.78749999999988773, 11.37500000000000000 ) ) ;
#8478 = ORIENTED_EDGE ( 'NONE', *, *, #12907, .T. ) ;
#8479 = CARTESIAN_POINT ( 'NONE',  ( 13.15909340670060956, 78.53732640481597116, -3.027695048772149455 ) ) ;
#8480 = DIRECTION ( 'NONE',  ( 0.000000000000000000, 0.000000000000000000, -1.000000000000000000 ) ) ;
#8481 = CARTESIAN_POINT ( 'NONE',  ( 7.500000000000002665, -27.73865070282584000, -2.034160311361948636 ) ) ;
#8482 = CARTESIAN_POINT ( 'NONE',  ( 13.26538156545109715, 72.34104678837115898, 2.525128613255597898 ) ) ;
#8483 = CARTESIAN_POINT ( 'NONE',  ( 2.425613699440361870, 79.09278513441491043, -13.28036210628224545 ) ) ;
#8484 = CARTESIAN_POINT ( 'NONE',  ( 10.92172942406179104, -13.26999999999999780, -7.935100905948385908 ) ) ;
#8485 = CARTESIAN_POINT ( 'NONE',  ( 13.49999999999999822, 63.28000000000000114, 4.386415899144237684 ) ) ;
#8486 = CARTESIAN_POINT ( 'NONE',  ( -13.47760860327369770, 52.90318445468975739, -0.7773389074900003415 ) ) ;
#8487 = CARTESIAN_POINT ( 'NONE',  ( 11.76794919243112325, 37.28000000000000114, 3.823638476888996607 ) ) ;
#8488 = CARTESIAN_POINT ( 'NONE',  ( -4.171729424061787483, 57.32999999999999829, -12.83926296998457417 ) ) ;
#8489 = DIRECTION ( 'NONE',  ( 1.000000000000000000, -6.302562568933760152E-16, 0.000000000000000000 ) ) ;
#8490 = CARTESIAN_POINT ( 'NONE',  ( -11.76794919243112325, -4.919999999999999041, 3.823638476888994386 ) ) ;
#8491 = CARTESIAN_POINT ( 'NONE',  ( 10.59389018096545598, 69.11125758787252948, 8.370637211927217436 ) ) ;
#8492 = CARTESIAN_POINT ( 'NONE',  ( -4.025229608893389432, 37.32472329120690802, -12.88605937129256240 ) ) ;
#8493 = CARTESIAN_POINT ( 'NONE',  ( 1.551971865843149168, 35.73580183865620086, 13.41075256337061994 ) ) ;
#8494 = CARTESIAN_POINT ( 'NONE',  ( -13.16986379960055409, -67.60624999999984652, 13.16986379959834252 ) ) ;
#8495 = CARTESIAN_POINT ( 'NONE',  ( -13.47478197652914744, 73.95848700326827441, 0.8248428433375331048 ) ) ;
#8496 = CARTESIAN_POINT ( 'NONE',  ( -2.473062413272049120, 76.26891320680448416, -13.27157550910005490 ) ) ;
#8497 = CARTESIAN_POINT ( 'NONE',  ( -0.3535656791965650081, 8.055112074840376835, -18.02368563757054432 ) ) ;
#8498 = LINE ( 'NONE', #14998, #11744 ) ;
#8499 = FACE_OUTER_BOUND ( 'NONE', #11335, .T. ) ;
#8500 = CARTESIAN_POINT ( 'NONE',  ( -8.343458848123582072, 30.38000000000000611, 11.48378591275254124 ) ) ;
#8501 = CARTESIAN_POINT ( 'NONE',  ( 9.520470885617715595, -6.869999999999993889, 6.917026985038135400 ) ) ;
#8502 = ADVANCED_FACE ( 'NONE', ( #3663 ), #4821, .T. ) ;
#8503 = CARTESIAN_POINT ( 'NONE',  ( -3.636496289402155746, 42.53000000000000114, 11.19198476289190936 ) ) ;
#8504 = CARTESIAN_POINT ( 'NONE',  ( 7.416407864998740607, 6.013974596215558854, -10.20780970022447676 ) ) ;
#8505 = CARTESIAN_POINT ( 'NONE',  ( -4.877653597743472957, 32.50418107437187842, 12.58959954281929683 ) ) ;
#8506 = CARTESIAN_POINT ( 'NONE',  ( 13.42353994245471149, 75.48170283343853271, -1.486489711945228942 ) ) ;
#8507 = CARTESIAN_POINT ( 'NONE',  ( 18.28134285175915252, 8.384379708534145006E-15, -3.505973352197490733 ) ) ;
#8508 = DIRECTION ( 'NONE',  ( 0.000000000000000000, -1.000000000000000000, 0.000000000000000000 ) ) ;
#8509 = CARTESIAN_POINT ( 'NONE',  ( 10.92172942406178926, 80.13000000000000966, 7.935100905948387684 ) ) ;
#8510 = PRODUCT_DEFINITION_FORMATION_WITH_SPECIFIED_SOURCE ( 'ANY', '', #16206, .NOT_KNOWN. ) ;
#8511 = CARTESIAN_POINT ( 'NONE',  ( 4.226080210030811912, 52.02818700926958684, -12.82458535216174234 ) ) ;
#8512 = CARTESIAN_POINT ( 'NONE',  ( -4.231956850230545797, 38.52784562378656830, 12.81957946664639003 ) ) ;
#8513 = CARTESIAN_POINT ( 'NONE',  ( 5.747437457432605257, 36.97097174469260494, -12.21544146112736406 ) ) ;
#8514 = CARTESIAN_POINT ( 'NONE',  ( -12.00000000000002842, 1.063974596215591317, -2.718289652585047788E-15 ) ) ;
#8515 = CARTESIAN_POINT ( 'NONE',  ( -4.638092529099512085, 49.34696448392821111, -12.67954046638503307 ) ) ;
#8516 = CARTESIAN_POINT ( 'NONE',  ( 11.58098153987704038, 63.17143452739731657, 6.937646968679790582 ) ) ;
#8517 = CARTESIAN_POINT ( 'NONE',  ( 13.47601834983935731, 42.40223155771326446, 0.8051276974000854958 ) ) ;
#8518 = CARTESIAN_POINT ( 'NONE',  ( -19.00000000000001776, 7.773118517290098950, 1.732050807568674466 ) ) ;
#8519 = CARTESIAN_POINT ( 'NONE',  ( 9.520470885617717371, 26.73000000000000398, -6.917026985038131848 ) ) ;
#8520 = VERTEX_POINT ( 'NONE', #15930 ) ;
#8521 = CARTESIAN_POINT ( 'NONE',  ( -7.272992578804310604, 66.37999999999999545, 10.01041549318726886 ) ) ;
#8522 = PLANE ( 'NONE',  #2311 ) ;
#8523 = CARTESIAN_POINT ( 'NONE',  ( 11.37500000000039435, -34.34062499999991758, -4.711679271993003404 ) ) ;
#8524 = CARTESIAN_POINT ( 'NONE',  ( 2.621994543952811015E-15, 10.18000000000000327, -14.19474002721660355 ) ) ;
#8525 = EDGE_LOOP ( 'NONE', ( #14331, #17421 ) ) ;
#8526 = ADVANCED_FACE ( 'NONE', ( #15752 ), #6327, .F. ) ;
#8527 = CARTESIAN_POINT ( 'NONE',  ( -12.47476134584739604, 43.74194706654176201, -5.166698879916627796 ) ) ;
#8528 = CARTESIAN_POINT ( 'NONE',  ( -7.500000000000000000, 106.5829119071944575, -7.723695278929459285 ) ) ;
#8529 =( BOUNDED_CURVE ( )  B_SPLINE_CURVE ( 2, ( #14776, #10825, #6765, #17357, #5270, #12143, #2489, #8010, #14515, #9077, #7921, #10655, #2319 ),
 .UNSPECIFIED., .F., .F. ) 
 B_SPLINE_CURVE_WITH_KNOTS ( ( 3, 2, 2, 2, 2, 2, 3 ),
 ( 0.1527777777777777624, 0.1555555555555555580, 0.1611111111111111216, 0.1666666666666666574, 0.1722222222222222210, 0.1777777777777777846, 0.1805555555555555525 ),
 .UNSPECIFIED. ) 
 CURVE ( )  GEOMETRIC_REPRESENTATION_ITEM ( )  RATIONAL_B_SPLINE_CURVE ( ( 0.9755282581475765991, 0.9755282581475765991, 1.000000000000000000, 0.9510565162951535312, 1.000000000000000000, 0.9510565162951535312, 1.000000000000000000, 0.9510565162951535312, 1.000000000000000000, 0.9510565162951535312, 1.000000000000000000, 0.9755282581475768211, 0.9755282581475768211 ) ) 
 REPRESENTATION_ITEM ( '' )  );
#8530 = CARTESIAN_POINT ( 'NONE',  ( -13.49999999999999822, -0.2200000000000017775, -4.386415899144240349 ) ) ;
#8531 = DIRECTION ( 'NONE',  ( 0.000000000000000000, 0.000000000000000000, 1.000000000000000000 ) ) ;
#8532 = CARTESIAN_POINT ( 'NONE',  ( 12.78284368098255541, 66.27342296526084908, 4.345939930100551685 ) ) ;
#8533 = CARTESIAN_POINT ( 'NONE',  ( 7.543221400131883136, 56.96276011477866774, 11.19924875908237460 ) ) ;
#8534 = CARTESIAN_POINT ( 'NONE',  ( 9.520470885617715595, 58.13000000000000256, 6.917026985038134512 ) ) ;
#8535 = CARTESIAN_POINT ( 'NONE',  ( -7.272992578804307939, 71.48000000000000398, -10.01041549318726886 ) ) ;
#8536 = CARTESIAN_POINT ( 'NONE',  ( -11.46833886424943572, 46.66385032393301913, -7.122929392610004129 ) ) ;
#8537 = CARTESIAN_POINT ( 'NONE',  ( 9.002869684684736029, 45.83076699320872649, -10.06118444092847675 ) ) ;
#8538 = CARTESIAN_POINT ( 'NONE',  ( -3.320475467054404886E-07, 70.18000001193918536, -13.49999999999999467 ) ) ;
#8539 =( LENGTH_UNIT ( ) NAMED_UNIT ( * ) SI_UNIT ( .MILLI., .METRE. ) );
#8540 = CARTESIAN_POINT ( 'NONE',  ( 10.17545303761933084, 30.77154226042120300, -8.873128808189237660 ) ) ;
#8541 = CARTESIAN_POINT ( 'NONE',  ( -5.357411621921722045, 56.48603353374912217, 12.39176923702621735 ) ) ;
#8542 = CARTESIAN_POINT ( 'NONE',  ( -3.437742735893688728, 50.55636824846342137, 13.05557927389223494 ) ) ;
#8543 = CARTESIAN_POINT ( 'NONE',  ( 10.11142744917618508, 33.08470593442759622, 8.956104572044239376 ) ) ;
#8544 = CARTESIAN_POINT ( 'NONE',  ( -7.999999999999670486, 5.918584287042171432, -24.73863375370606477 ) ) ;
#8545 = CARTESIAN_POINT ( 'NONE',  ( -8.992807909601426175, 8.063463562524669115, -15.58762070717333970 ) ) ;
#8546 = ORIENTED_EDGE ( 'NONE', *, *, #6216, .F. ) ;
#8547 = CARTESIAN_POINT ( 'NONE',  ( -13.47511189851588931, 61.90170573638860674, -0.8193731989312416086 ) ) ;
#8548 = ORIENTED_EDGE ( 'NONE', *, *, #10569, .T. ) ;
#8549 = EDGE_CURVE ( 'NONE', #2603, #9217, #352, .T. ) ;
#8550 = CARTESIAN_POINT ( 'NONE',  ( 18.62500000000000000, -23.89999999999996305, 1.560692158462880521E-12 ) ) ;
#8551 = CARTESIAN_POINT ( 'NONE',  ( -13.45089070962791489, 43.97009932163807377, 1.157149274454969401 ) ) ;
#8552 = VECTOR ( 'NONE', #17041, 1000.000000000000000 ) ;
#8553 = CARTESIAN_POINT ( 'NONE',  ( 13.49999999999999822, 36.27999999999999403, 4.386415899144237684 ) ) ;
#8554 = CARTESIAN_POINT ( 'NONE',  ( -0.2540371354857682284, 46.18913186441219665, -13.49794113769755555 ) ) ;
#8555 = CARTESIAN_POINT ( 'NONE',  ( -10.09036394839171003, 67.58397492445097043, -8.968536542104889264 ) ) ;
#8556 = CARTESIAN_POINT ( 'NONE',  ( 18.62499999999935341, -91.60937499999975842, 7.714727599200469577 ) ) ;
#8557 = AXIS2_PLACEMENT_3D ( 'NONE', #30, #2929, #14857 ) ;
#8558 = CARTESIAN_POINT ( 'NONE',  ( 10.14209061328275752, 54.08650388490638505, 8.919889534789382068 ) ) ;
#8559 = ORIENTED_EDGE ( 'NONE', *, *, #5983, .T. ) ;
#8560 = CARTESIAN_POINT ( 'NONE',  ( -0.2710101708259924358, 64.18974430090325711, -13.49761915939118317 ) ) ;
#8561 = VERTEX_POINT ( 'NONE', #830 ) ;
#8562 = CARTESIAN_POINT ( 'NONE',  ( 5.339658159925267711, 66.98672795088741339, -12.39911587653581293 ) ) ;
#8563 = CARTESIAN_POINT ( 'NONE',  ( -3.202417373558799074, 34.29514631974450367, -13.11514094275671383 ) ) ;
#8564 = CARTESIAN_POINT ( 'NONE',  ( 11.37500000000000000, -66.59999999999983800, 9.531744055041752924E-13 ) ) ;
#8565 = CARTESIAN_POINT ( 'NONE',  ( 12.71205548718733702, 78.26577299247003339, 4.546657709176281870 ) ) ;
#8566 = CARTESIAN_POINT ( 'NONE',  ( -16.47733079524789090, 7.956441929884681130, 8.178053476329983695 ) ) ;
#8567 = CARTESIAN_POINT ( 'NONE',  ( 7.500000000000002665, -27.80914044117234596, 0.5315352956498873294 ) ) ;
#8568 = CARTESIAN_POINT ( 'NONE',  ( 11.46276161444878383, 72.16349900300471631, 7.131289053549557444 ) ) ;
#8569 = CARTESIAN_POINT ( 'NONE',  ( 7.272992578804308828, 31.98000000000000043, 10.01041549318726709 ) ) ;
#8570 = CARTESIAN_POINT ( 'NONE',  ( -13.49999999999999822, 64.78000000000000114, -4.386415899144240349 ) ) ;
#8571 = CARTESIAN_POINT ( 'NONE',  ( -2.527007466902615462, 52.27086174099205351, -13.26155452052046080 ) ) ;
#8572 = VECTOR ( 'NONE', #4784, 1000.000000000000000 ) ;
#8573 = CARTESIAN_POINT ( 'NONE',  ( -9.520470885617717371, 39.23000000000000398, 6.917026985038133624 ) ) ;
#8574 = CARTESIAN_POINT ( 'NONE',  ( 13.50000000000000000, 53.43000000000000682, 1.653273178848926867E-15 ) ) ;
#8575 = CARTESIAN_POINT ( 'NONE',  ( 0.000000000000000000, -22.00000000000000000, 0.000000000000000000 ) ) ;
#8576 = EDGE_CURVE ( 'NONE', #13571, #9800, #2594, .T. ) ;
#8577 = CARTESIAN_POINT ( 'NONE',  ( 9.520470885617715595, -0.8699999999999957767, 6.917026985038135400 ) ) ;
#8578 = CARTESIAN_POINT ( 'NONE',  ( 11.63057281378106289, 69.17483938076107108, 6.854191306154013397 ) ) ;
#8579 = CARTESIAN_POINT ( 'NONE',  ( 3.708203932499376076, 1.963974596215575019, 11.41267819554186680 ) ) ;
#8580 = CARTESIAN_POINT ( 'NONE',  ( -10.92172942406179104, 79.23000000000000398, 7.935100905948387684 ) ) ;
#8581 = CARTESIAN_POINT ( 'NONE',  ( -7.714727599200466912, -101.9468749999998067, 18.62499999999935341 ) ) ;
#8582 = CARTESIAN_POINT ( 'NONE',  ( -13.46249943993917775, 73.96494795259233967, 1.009710742264189332 ) ) ;
#8583 = LINE ( 'NONE', #13934, #12046 ) ;
#8584 = CARTESIAN_POINT ( 'NONE',  ( 1.900613283894418970, 8.969143981464171134, -12.00000000000000711 ) ) ;
#8585 = FACE_OUTER_BOUND ( 'NONE', #10146, .T. ) ;
#8586 = CYLINDRICAL_SURFACE ( 'NONE', #12513, 13.50000000000000000 ) ;
#8587 = LINE ( 'NONE', #6995, #446 ) ;
#8588 = CARTESIAN_POINT ( 'NONE',  ( -11.76794919243112325, -11.06999999999999673, -2.602085213965210642E-15 ) ) ;
#8589 = CARTESIAN_POINT ( 'NONE',  ( -7.272992578804307939, 35.47999999999999687, -10.01041549318727064 ) ) ;
#8590 = CARTESIAN_POINT ( 'NONE',  ( 6.750022565184456980, -18.07073825016061619, 11.69132992304556673 ) ) ;
#8591 = CARTESIAN_POINT ( 'NONE',  ( -11.23704444756839216, 32.21100520952357016, 7.482062774987143783 ) ) ;
#8592 = CARTESIAN_POINT ( 'NONE',  ( 6.301401044479416846, 74.91092896658807376, 11.94220124380246162 ) ) ;
#8593 = CARTESIAN_POINT ( 'NONE',  ( -8.891200544363830713E-16, 2.680000000000005045, 13.49999999999999822 ) ) ;
#8594 = CARTESIAN_POINT ( 'NONE',  ( -13.50000000000000000, 81.93000000000000682, -3.306546357697853733E-15 ) ) ;
#8595 = CARTESIAN_POINT ( 'NONE',  ( 0.8749885751862738203, 52.14854123505212158, -13.47204428328692849 ) ) ;
#8596 = EDGE_CURVE ( 'NONE', #6661, #5891, #2486, .T. ) ;
#8597 = CARTESIAN_POINT ( 'NONE',  ( 7.347880794884122694E-16, 0.000000000000000000, -20.00000000000000000 ) ) ;
#8598 = CARTESIAN_POINT ( 'NONE',  ( 0.3867960985429125254, 37.16609886577710853, -13.49524483310550060 ) ) ;
#8599 = CARTESIAN_POINT ( 'NONE',  ( -7.500000000000000000, 98.93000000000002103, -8.999999999999996447 ) ) ;
#8600 = CARTESIAN_POINT ( 'NONE',  ( -3.695260882689679338, 49.31284492995563795, -12.98818747258629536 ) ) ;
#8601 = CARTESIAN_POINT ( 'NONE',  ( 2.626233336093215076, 62.77444219063707465, 13.24209077638737675 ) ) ;
#8602 = LINE ( 'NONE', #6204, #13608 ) ;
#8603 = CARTESIAN_POINT ( 'NONE',  ( 8.545810036750047800, 48.85228211165327394, -10.45080393046335132 ) ) ;
#8604 = CARTESIAN_POINT ( 'NONE',  ( -9.520470885617715595, 18.63000000000000611, -6.917026985038136289 ) ) ;
#8605 = VERTEX_POINT ( 'NONE', #10396 ) ;
#8606 = CARTESIAN_POINT ( 'NONE',  ( -11.76794919243112325, 65.93000000000000682, -2.882316262207890869E-15 ) ) ;
#8607 = CARTESIAN_POINT ( 'NONE',  ( 4.711679271994911211, -12.52187499999995524, -11.37499999999960743 ) ) ;
#8608 = CARTESIAN_POINT ( 'NONE',  ( -9.552639591052204498E-13, -79.08749999999980673, 11.37500000000000000 ) ) ;
#8609 = CARTESIAN_POINT ( 'NONE',  ( 13.50000000000000355, 3.580000000000008953, -4.386415899144233244 ) ) ;
#8610 = ORIENTED_EDGE ( 'NONE', *, *, #17286, .F. ) ;
#8611 = CARTESIAN_POINT ( 'NONE',  ( -0.4867513977796573132, 43.19750178289612563, -13.49122469273548575 ) ) ;
#8612 = DIRECTION ( 'NONE',  ( 0.000000000000000000, -1.000000000000000000, 0.000000000000000000 ) ) ;
#8613 = CARTESIAN_POINT ( 'NONE',  ( 13.50000000000000000, 1.430000000000014593, 1.734723475976807094E-15 ) ) ;
#8614 = CARTESIAN_POINT ( 'NONE',  ( 1.561832610794586538E-12, -4.162499999999989875, -18.62500000000000000 ) ) ;
#8615 = CARTESIAN_POINT ( 'NONE',  ( 5.757975047644410260, 65.88943174946119541, 12.21048708421974816 ) ) ;
#8616 = CARTESIAN_POINT ( 'NONE',  ( -13.50000000000000000, 79.93000000000000682, -3.306546357697853733E-15 ) ) ;
#8617 = CARTESIAN_POINT ( 'NONE',  ( -3.636496289402155746, 60.53000000000000114, 11.19198476289190936 ) ) ;
#8618 = CARTESIAN_POINT ( 'NONE',  ( 11.76794919243112325, 58.28000000000000114, 3.823638476888996607 ) ) ;
#8619 = CARTESIAN_POINT ( 'NONE',  ( -11.32173173042431991, 46.65434610059125475, -7.353121830783978297 ) ) ;
#8620 = CARTESIAN_POINT ( 'NONE',  ( 10.63213266513623978, 45.74654076961098070, -8.319152667901684950 ) ) ;
#8621 = CARTESIAN_POINT ( 'NONE',  ( 7.721945602315970270, 69.88954231929918137, -11.07992460466698681 ) ) ;
#8622 = EDGE_CURVE ( 'NONE', #3432, #5466, #11130, .T. ) ;
#8623 =( LENGTH_UNIT ( ) NAMED_UNIT ( * ) SI_UNIT ( .MILLI., .METRE. ) );
#8624 = CARTESIAN_POINT ( 'NONE',  ( 6.449393272122638798, 30.94317789798385121, -11.86697286938268725 ) ) ;
#8625 = CARTESIAN_POINT ( 'NONE',  ( -13.38148664391157361, 55.99414316929159696, 1.834830169894675844 ) ) ;
#8626 = DIRECTION ( 'NONE',  ( 0.000000000000000000, 0.000000000000000000, -1.000000000000000000 ) ) ;
#8627 = VECTOR ( 'NONE', #6340, 1000.000000000000000 ) ;
#8628 = CARTESIAN_POINT ( 'NONE',  ( 1.628308837847167748E-06, 32.68004529479373588, 13.49999999999980460 ) ) ;
#8629 = CARTESIAN_POINT ( 'NONE',  ( -0.5902394228252099140, 73.20122283213095216, -13.49999999999999289 ) ) ;
#8630 = CARTESIAN_POINT ( 'NONE',  ( 9.828641339704693891, 39.78975999636411132, -9.256972243478518436 ) ) ;
#8631 = ORIENTED_EDGE ( 'NONE', *, *, #4346, .F. ) ;
#8632 = CARTESIAN_POINT ( 'NONE',  ( -12.74970089692343045, 62.09010389230079596, 4.438088001292920026 ) ) ;
#8633 =( BOUNDED_CURVE ( )  B_SPLINE_CURVE ( 2, ( #9481, #2896, #8241, #5496, #14827, #1581, #14658, #12027, #1316, #8149, #268, #2546, #7975 ),
 .UNSPECIFIED., .F., .T. ) 
 B_SPLINE_CURVE_WITH_KNOTS ( ( 3, 2, 2, 2, 2, 2, 3 ),
 ( 0.9027777777777777901, 0.9055555555555555580, 0.9111111111111110938, 0.9166666666666666297, 0.9222222222222222765, 0.9277777777777778123, 0.9305555555555555802 ),
 .UNSPECIFIED. ) 
 CURVE ( )  GEOMETRIC_REPRESENTATION_ITEM ( )  RATIONAL_B_SPLINE_CURVE ( ( 0.9755282581475768211, 0.9755282581475768211, 1.000000000000000000, 0.9510565162951535312, 1.000000000000000000, 0.9510565162951535312, 1.000000000000000000, 0.9510565162951535312, 1.000000000000000000, 0.9510565162951535312, 1.000000000000000000, 0.9755282581475768211, 0.9755282581475768211 ) ) 
 REPRESENTATION_ITEM ( '' )  );
#8634 = ORIENTED_EDGE ( 'NONE', *, *, #9164, .F. ) ;
#8635 = CARTESIAN_POINT ( 'NONE',  ( 10.92172942406178926, 33.13000000000002387, 7.935100905948385908 ) ) ;
#8636 = CARTESIAN_POINT ( 'NONE',  ( -18.62499999999935341, -81.13437499999982094, -7.714727599200458030 ) ) ;
#8637 = CARTESIAN_POINT ( 'NONE',  ( 9.670042864717805386, 48.06219784168897036, 9.420394723061004782 ) ) ;
#8638 = CARTESIAN_POINT ( 'NONE',  ( 8.378362625313673817, -1.749711886770878784E-15, 10.58551083881864407 ) ) ;
#8639 = CARTESIAN_POINT ( 'NONE',  ( -10.92172942406178926, 37.62999999999999545, -7.935100905948389460 ) ) ;
#8640 = CARTESIAN_POINT ( 'NONE',  ( -8.343458848123576743, 42.47999999999999687, -11.48378591275254301 ) ) ;
#8641 = CARTESIAN_POINT ( 'NONE',  ( -7.112170435543458069, 46.44454114888061724, -11.48319410635906479 ) ) ;
#8642 = CARTESIAN_POINT ( 'NONE',  ( -7.930396875273861390, 67.47978613725511821, -10.92539274502803259 ) ) ;
#8643 = CARTESIAN_POINT ( 'NONE',  ( -11.37500000000000178, -1.074999999999978639, -9.545674412382054647E-13 ) ) ;
#8644 = CARTESIAN_POINT ( 'NONE',  ( 5.585949171536172209, 53.88247118449140061, 12.30201563545229781 ) ) ;
#8645 = ORIENTED_EDGE ( 'NONE', *, *, #17130, .T. ) ;
#8646 = CARTESIAN_POINT ( 'NONE',  ( -8.208207767219146689, 64.49222101755708536, -10.71938957358478461 ) ) ;
#8647 = ORIENTED_EDGE ( 'NONE', *, *, #9376, .F. ) ;
#8648 = CARTESIAN_POINT ( 'NONE',  ( 10.92172942406179104, 9.730000000000016414, -7.935100905948385908 ) ) ;
#8649 = CARTESIAN_POINT ( 'NONE',  ( -7.797167812233946727, 34.47380972907037489, -11.02479444021394350 ) ) ;
#8650 = CARTESIAN_POINT ( 'NONE',  ( 4.711679271993006068, -30.17812499999993747, 11.37500000000039257 ) ) ;
#8651 = CARTESIAN_POINT ( 'NONE',  ( 9.010525653276635794, 78.02962374744581098, 10.05410809128824745 ) ) ;
#8652 = CARTESIAN_POINT ( 'NONE',  ( 1.753268986668952691E-06, 80.68004880551006863, 13.49999999999977263 ) ) ;
#8653 = DIRECTION ( 'NONE',  ( 0.000000000000000000, 0.000000000000000000, 1.000000000000000000 ) ) ;
#8654 = CARTESIAN_POINT ( 'NONE',  ( 1.469576158976824144E-15, -22.00000000000000000, -12.00000000000000178 ) ) ;
#8655 = CARTESIAN_POINT ( 'NONE',  ( 12.94854022286095763, 72.56673908956170749, -3.819461041215378660 ) ) ;
#8656 = CARTESIAN_POINT ( 'NONE',  ( 9.520470885617717371, 29.73000000000000753, -6.917026985038131848 ) ) ;
#8657=STYLED_ITEM('',(#17526),#3260);
#8658 = CARTESIAN_POINT ( 'NONE',  ( 4.171729424061791924, 67.03000000000000114, -12.83926296998457239 ) ) ;
#8659 = CARTESIAN_POINT ( 'NONE',  ( -7.714235717713363805, 52.46982633924920947, -11.10504961456102357 ) ) ;
#8660 = CARTESIAN_POINT ( 'NONE',  ( 2.272985001014427788E-15, 41.17999999999999972, -12.37355403259654985 ) ) ;
#8661 = CARTESIAN_POINT ( 'NONE',  ( -9.520470885617717371, -13.76999999999999780, 6.917026985038133624 ) ) ;
#8662 = CARTESIAN_POINT ( 'NONE',  ( 13.50000000000000355, 53.57999999999999829, -4.386415899144233244 ) ) ;
#8663 = CARTESIAN_POINT ( 'NONE',  ( 0.9450715873491259966, 50.71399393198645811, 13.47525569251407518 ) ) ;
#8664 = CARTESIAN_POINT ( 'NONE',  ( -7.272992578804307939, -5.520000000000001350, -10.01041549318726886 ) ) ;
#8665 = CARTESIAN_POINT ( 'NONE',  ( 5.110268676760429507, 68.86456870269141461, 12.49542038485116535 ) ) ;
#8666 = CARTESIAN_POINT ( 'NONE',  ( -18.62499999999934985, -7.284374999999982947, -7.714727599200458918 ) ) ;
#8667 = CARTESIAN_POINT ( 'NONE',  ( -8.891200544363830713E-16, 70.68000000000000682, 13.50000000000000000 ) ) ;
#8668 = CARTESIAN_POINT ( 'NONE',  ( 7.714727599200456254, -60.32187499999988489, -18.62499999999935341 ) ) ;
#8669 = CARTESIAN_POINT ( 'NONE',  ( -13.42711900164165861, 73.88114203177188699, -1.405880853923186180 ) ) ;
#8670 = AXIS2_PLACEMENT_3D ( 'NONE', #14156, #15475, #4549 ) ;
#8671 = CARTESIAN_POINT ( 'NONE',  ( -9.171191987446322358, 76.53731527584839966, -9.908219757055420018 ) ) ;
#8672 = CARTESIAN_POINT ( 'NONE',  ( -1.545162525932825686E-06, 79.18000005555833809, -13.49999999999990941 ) ) ;
#8673 = CARTESIAN_POINT ( 'NONE',  ( 0.000000000000000000, 80.93000000000000682, 0.000000000000000000 ) ) ;
#8674 = DIRECTION ( 'NONE',  ( 0.000000000000000000, 1.000000000000000000, 0.000000000000000000 ) ) ;
#8675 = CARTESIAN_POINT ( 'NONE',  ( -7.272992578804310604, -4.620000000000000995, 10.01041549318726709 ) ) ;
#8676 = CARTESIAN_POINT ( 'NONE',  ( -9.520470885617717371, 42.22999999999999687, 6.917026985038133624 ) ) ;
#8677 = CARTESIAN_POINT ( 'NONE',  ( -8.992656840795357098, 32.33142381460860548, 10.07316879344405791 ) ) ;
#8678 = CARTESIAN_POINT ( 'NONE',  ( 1.328803061132558749, 74.72777884802709991, 13.43444388716402038 ) ) ;
#8679 = EDGE_CURVE ( 'NONE', #3801, #8975, #16621, .T. ) ;
#8680 = CARTESIAN_POINT ( 'NONE',  ( -0.2851956912289982382, 53.66974537925386102, 13.49700562860493314 ) ) ;
#8681 = CARTESIAN_POINT ( 'NONE',  ( -7.272992578804307939, 32.47999999999999687, -10.01041549318726886 ) ) ;
#8682 = CARTESIAN_POINT ( 'NONE',  ( 3.968858122459704152, 52.03755112169107377, -12.90597491634626870 ) ) ;
#8683 = CARTESIAN_POINT ( 'NONE',  ( -4.870330804223598875, 38.50445280852472507, 12.59249463255201462 ) ) ;
#8684 = CARTESIAN_POINT ( 'NONE',  ( 5.672580605102411688, 36.97381777227605681, -12.25043497061033015 ) ) ;
#8685 = DIRECTION ( 'NONE',  ( 0.000000000000000000, 0.000000000000000000, 1.000000000000000000 ) ) ;
#8686 = PLANE ( 'NONE',  #4997 ) ;
#8687 = CARTESIAN_POINT ( 'NONE',  ( 10.21212867364205046, 63.09039058033595637, 8.832471590444903597 ) ) ;
#8688 = CARTESIAN_POINT ( 'NONE',  ( 6.884270893848766448, 41.93466036346448789, 11.62526077269765601 ) ) ;
#8689 = CARTESIAN_POINT ( 'NONE',  ( 11.58339546198362591, 48.68871274354637535, -6.950020419437135111 ) ) ;
#8690 = CARTESIAN_POINT ( 'NONE',  ( 3.636496289402154414, 19.83000000000001251, 11.19198476289190758 ) ) ;
#8691 = ORIENTED_EDGE ( 'NONE', *, *, #15210, .T. ) ;
#8692 = CARTESIAN_POINT ( 'NONE',  ( -7.272992578804307939, 71.48000000000000398, -10.01041549318727064 ) ) ;
#8693 = CARTESIAN_POINT ( 'NONE',  ( 8.043339635997652337, -11.48124999999995488, -8.043339635996304082 ) ) ;
#8694 = CARTESIAN_POINT ( 'NONE',  ( 4.711679271993006068, -30.17812499999993037, 11.37500000000039257 ) ) ;
#8695 = CARTESIAN_POINT ( 'NONE',  ( -10.92172942406179104, 5.230000000000012861, 7.935100905948385908 ) ) ;
#8696 = CARTESIAN_POINT ( 'NONE',  ( -7.272992578804307939, 33.47999999999999687, -10.01041549318726886 ) ) ;
#8697 = DIRECTION ( 'NONE',  ( -0.000000000000000000, 1.000000000000000000, -0.000000000000000000 ) ) ;
#8698 = CARTESIAN_POINT ( 'NONE',  ( -10.92172942406179104, 6.230000000000012861, 7.935100905948385908 ) ) ;
#8699 = CARTESIAN_POINT ( 'NONE',  ( 7.714727599197339636, -46.82812499999987921, 18.62500000000063949 ) ) ;
#8700 = CARTESIAN_POINT ( 'NONE',  ( 8.134860252326546970, 65.98893604550748648, 10.77385971222135552 ) ) ;
#8701 = CARTESIAN_POINT ( 'NONE',  ( 17.42428528562858148, 0.000000000000000000, -19.29752010712846300 ) ) ;
#8702 = CARTESIAN_POINT ( 'NONE',  ( -11.76794919243112325, 53.77999999999999403, -3.823638476888998827 ) ) ;
#8703 = CARTESIAN_POINT ( 'NONE',  ( -13.49999999999999822, 34.07999999999999829, 4.386415899144235908 ) ) ;
#8704 = CARTESIAN_POINT ( 'NONE',  ( -11.76794919243112325, 59.77999999999998693, -3.823638476888998827 ) ) ;
#8705 = CARTESIAN_POINT ( 'NONE',  ( -9.913970262008090728, 46.57449140322882641, -9.165228541796420103 ) ) ;
#8706 =( REPRESENTATION_RELATIONSHIP ('NONE','NONE', #7275, #5468 ) REPRESENTATION_RELATIONSHIP_WITH_TRANSFORMATION ( #2268 )SHAPE_REPRESENTATION_RELATIONSHIP( ) );
#8707 = CARTESIAN_POINT ( 'NONE',  ( 10.67523966630402121, 45.74411538286880585, -8.263863657552700914 ) ) ;
#8708 = CARTESIAN_POINT ( 'NONE',  ( 5.565866721395538619, 69.97797074884671531, -12.29937346137027632 ) ) ;
#8709 = CARTESIAN_POINT ( 'NONE',  ( 1.832901445459844014, 31.11425710500970254, -13.38003086484803106 ) ) ;
#8710 = CARTESIAN_POINT ( 'NONE',  ( -10.58832603877217871, 56.24920692690567137, 8.377620954876409343 ) ) ;
#8711 = DIRECTION ( 'NONE',  ( 0.000000000000000000, -1.000000000000000000, 0.000000000000000000 ) ) ;
#8712 = CARTESIAN_POINT ( 'NONE',  ( 9.818219314833713796, 33.06951371705229548, 9.274956680371715834 ) ) ;
#8713 = CARTESIAN_POINT ( 'NONE',  ( 4.083253397203186807, 43.03321070571565343, -12.86830022185737477 ) ) ;
#8714 = CARTESIAN_POINT ( 'NONE',  ( 8.099268731515945063, 39.87266764020058218, -10.80082015226388314 ) ) ;
#8715 = ORIENTED_EDGE ( 'NONE', *, *, #1763, .F. ) ;
#8716 = CARTESIAN_POINT ( 'NONE',  ( -11.14572871157717593, 62.21664499426510275, 7.617379339931979132 ) ) ;
#8717 = ORIENTED_EDGE ( 'NONE', *, *, #10666, .F. ) ;
#8718 = CARTESIAN_POINT ( 'NONE',  ( -10.92172942406179104, 32.23000000000001108, 7.935100905948385908 ) ) ;
#8719 = CARTESIAN_POINT ( 'NONE',  ( 18.62500000000064304, -17.69062499999995453, -7.714727599197335195 ) ) ;
#8720 = EDGE_CURVE ( 'NONE', #14307, #5870, #2866, .T. ) ;
#8721 = CARTESIAN_POINT ( 'NONE',  ( 7.053763874080417828, 47.94203897529205705, 11.51277963570407792 ) ) ;
#8722 = CARTESIAN_POINT ( 'NONE',  ( 4.049944587781194372, 58.03463076063811599, -12.88329806241152298 ) ) ;
#8723 = CARTESIAN_POINT ( 'NONE',  ( -13.50000000000000000, 31.92999999999999972, -3.306546357697853733E-15 ) ) ;
#8724 = CARTESIAN_POINT ( 'NONE',  ( 4.171729424061791924, 42.03000000000000114, -12.83926296998457239 ) ) ;
#8725 = CARTESIAN_POINT ( 'NONE',  ( 12.11540212872241007, -1.688490311990081981E-15, 5.028035910480880943 ) ) ;
#8726 = AXIS2_PLACEMENT_3D ( 'NONE', #5746, #4407, #8314 ) ;
#8727 = DIRECTION ( 'NONE',  ( 1.000000000000000000, 0.000000000000000000, 0.000000000000000000 ) ) ;
#8728 = CARTESIAN_POINT ( 'NONE',  ( 17.32050807568873196, 0.000000000000000000, 10.00000000000008171 ) ) ;
#8729 = CARTESIAN_POINT ( 'NONE',  ( 11.37500000000039613, -10.44062499999995453, -4.711679271993004292 ) ) ;
#8730 = CARTESIAN_POINT ( 'NONE',  ( 10.70119226595359585, 54.11735038901769457, 8.230103751483696328 ) ) ;
#8731 = CARTESIAN_POINT ( 'NONE',  ( 9.520470885617717371, 14.72999999999999332, -6.917026985038131848 ) ) ;
#8732 = ORIENTED_EDGE ( 'NONE', *, *, #4932, .T. ) ;
#8733 = LINE ( 'NONE', #837, #5573 ) ;
#8734 = VERTEX_POINT ( 'NONE', #7050 ) ;
#8735 = CARTESIAN_POINT ( 'NONE',  ( 13.50000000000000000, 9.429999999999994387, 1.734723475976807094E-15 ) ) ;
#8736 = CARTESIAN_POINT ( 'NONE',  ( -3.526270707235371837, 34.30679044915609666, -13.03322718403512326 ) ) ;
#8737 = CARTESIAN_POINT ( 'NONE',  ( -11.37499999999960387, -90.53437499999978400, -4.711679271994910323 ) ) ;
#8738 = AXIS2_PLACEMENT_3D ( 'NONE', #8207, #1286, #12079 ) ;
#8739 = CARTESIAN_POINT ( 'NONE',  ( 9.433938897025715420, 78.05027556318721338, 9.660859765897237494 ) ) ;
#8740 = CARTESIAN_POINT ( 'NONE',  ( 2.138189944381242213, 48.10311857767972299, -13.49999999999999822 ) ) ;
#8741 = CARTESIAN_POINT ( 'NONE',  ( 17.14741290055379253, 7.815224843475954586, 8.000000000000085265 ) ) ;
#8742 = EDGE_CURVE ( 'NONE', #967, #8820, #3922, .T. ) ;
#8743 = CARTESIAN_POINT ( 'NONE',  ( -20.00000000000000000, 0.000000000000000000, -2.102236684100764122E-13 ) ) ;
#8744 = CARTESIAN_POINT ( 'NONE',  ( 12.97739931409362235, 72.56301366025002153, -3.719884340965235126 ) ) ;
#8745 = CARTESIAN_POINT ( 'NONE',  ( -9.520470885617717371, 31.23000000000000753, 6.917026985038133624 ) ) ;
#8746 = CARTESIAN_POINT ( 'NONE',  ( -13.49999999999999822, 62.07999999999999119, 4.386415899144235908 ) ) ;
#8747 = CARTESIAN_POINT ( 'NONE',  ( -5.127610894157791144, 52.36511171218869265, -12.49413350819052582 ) ) ;
#8748 = CARTESIAN_POINT ( 'NONE',  ( 9.520470885617717371, 40.72999999999999687, -6.917026985038131848 ) ) ;
#8749 = CARTESIAN_POINT ( 'NONE',  ( 2.279995255611139653E-15, -14.82000000000000384, -12.37355403259654985 ) ) ;
#8750 = CARTESIAN_POINT ( 'NONE',  ( 13.50000000000000000, 56.42999999999999972, 1.653273178848926867E-15 ) ) ;
#8751 = CARTESIAN_POINT ( 'NONE',  ( 10.92172942406179104, 77.73000000000000398, -7.935100905948385908 ) ) ;
#8752 = AXIS2_PLACEMENT_3D ( 'NONE', #6740, #5413, #5596 ) ;
#8753 = CARTESIAN_POINT ( 'NONE',  ( -7.272992578804307939, -2.520000000000001794, -10.01041549318726886 ) ) ;
#8754 = CARTESIAN_POINT ( 'NONE',  ( -4.574181969382655311, 68.51537738898377938, 12.70201094514906970 ) ) ;
#8755 = CARTESIAN_POINT ( 'NONE',  ( -18.62500000000000000, -41.62499999999990052, -1.562973063126292555E-12 ) ) ;
#8756 = CARTESIAN_POINT ( 'NONE',  ( -1.844924112955495524E-14, 72.18000000000000682, -13.50000000000000000 ) ) ;
#8757 = CARTESIAN_POINT ( 'NONE',  ( 18.62500000000064659, -74.89062499999985789, -7.714727599197336083 ) ) ;
#8758 = CARTESIAN_POINT ( 'NONE',  ( -13.46880766683457686, 73.96184857042898386, 0.9211851228833413119 ) ) ;
#8759 = LINE ( 'NONE', #4764, #12889 ) ;
#8760 = CARTESIAN_POINT ( 'NONE',  ( 18.99999999999999289, 0.000000000000000000, 1.732050807568941586 ) ) ;
#8761 = CARTESIAN_POINT ( 'NONE',  ( 8.402223690147334167, 8.016752490022669875, -16.11047477678861739 ) ) ;
#8762 = CARTESIAN_POINT ( 'NONE',  ( 8.343458848123583849, 25.88000000000000611, -11.48378591275253768 ) ) ;
#8763 = CARTESIAN_POINT ( 'NONE',  ( -7.576616670048093940E-16, 36.67999999999999972, 12.37355403259654807 ) ) ;
#8764 = EDGE_CURVE ( 'NONE', #1172, #2325, #14266, .T. ) ;
#8765 = CARTESIAN_POINT ( 'NONE',  ( -1.567828446471241755, 32.62365072876585970, 13.40870118950181400 ) ) ;
#8766 = CARTESIAN_POINT ( 'NONE',  ( -24.73863375370588003, 5.918584287042170544, -8.000000000000282441 ) ) ;
#8767 = VECTOR ( 'NONE', #10366, 1000.000000000000000 ) ;
#8768 = CARTESIAN_POINT ( 'NONE',  ( -0.3449943859400333435, 53.66759530121692734, 13.49560261416635498 ) ) ;
#8769 =( LENGTH_UNIT ( ) NAMED_UNIT ( * ) SI_UNIT ( .MILLI., .METRE. ) );
#8770 = CARTESIAN_POINT ( 'NONE',  ( 2.607531440858944223E-15, 81.18000000000000682, -14.19474002721660355 ) ) ;
#8771 = CARTESIAN_POINT ( 'NONE',  ( 13.14200413229988129, 51.53974922401104664, -3.092116881306331333 ) ) ;
#8772 = CARTESIAN_POINT ( 'NONE',  ( -7.051585598576367353, 38.41817575276711949, 11.51199000259391703 ) ) ;
#8773 = DIRECTION ( 'NONE',  ( 0.000000000000000000, 0.000000000000000000, 1.000000000000000000 ) ) ;
#8774 = CARTESIAN_POINT ( 'NONE',  ( 4.711679271994909435, -69.72187499999982663, -11.37499999999960387 ) ) ;
#8775 = CARTESIAN_POINT ( 'NONE',  ( 1.653273178848926472E-15, 80.93000000000000682, 13.50000000000000000 ) ) ;
#8776 = FACE_BOUND ( 'NONE', #9238, .T. ) ;
#8777 = CARTESIAN_POINT ( 'NONE',  ( 0.2771608746823925329, 62.68996565959619716, 13.49715969379329472 ) ) ;
#8778 = DIRECTION ( 'NONE',  ( 0.000000000000000000, -1.000000000000000000, 0.000000000000000000 ) ) ;
#8779 = CARTESIAN_POINT ( 'NONE',  ( 13.23997872644318896, 48.52304506666694550, -2.636916081698648107 ) ) ;
#8780 = CARTESIAN_POINT ( 'NONE',  ( -11.76794919243112325, 24.93000000000000682, -2.602085213965210642E-15 ) ) ;
#8781 = VERTEX_POINT ( 'NONE', #12947 ) ;
#8782 = CARTESIAN_POINT ( 'NONE',  ( -7.272992578804310604, 69.37999999999999545, 10.01041549318726886 ) ) ;
#8783 = CARTESIAN_POINT ( 'NONE',  ( -13.16986379959834252, -82.24374999999977831, -13.16986379960055409 ) ) ;
#8784 = CARTESIAN_POINT ( 'NONE',  ( -4.711679271993003404, -38.50312499999991189, -11.37500000000039435 ) ) ;
#8785 = CARTESIAN_POINT ( 'NONE',  ( -0.9595081608899134196, 43.21449727781597971, -13.46834895437819135 ) ) ;
#8786 = CARTESIAN_POINT ( 'NONE',  ( -2.648919002459650063, 80.92999999999994998, -12.65678160791745022 ) ) ;
#8787 = CARTESIAN_POINT ( 'NONE',  ( -18.62500000000000000, -74.92499999999982663, -1.562973063126292555E-12 ) ) ;
#8788 = CARTESIAN_POINT ( 'NONE',  ( -1.732050807568877859, 7.773118517290099838, -18.99999999999999645 ) ) ;
#8789 = CARTESIAN_POINT ( 'NONE',  ( -11.76794919243112325, 50.92999999999999972, -2.882316262207890869E-15 ) ) ;
#8790 = DIRECTION ( 'NONE',  ( 0.8660254037844332675, -0.000000000000000000, 0.5000000000000092149 ) ) ;
#8791 = CARTESIAN_POINT ( 'NONE',  ( -12.04654261135511639, 59.15468403854464441, 6.098114165576594914 ) ) ;
#8792 = CARTESIAN_POINT ( 'NONE',  ( 12.88012409951591586, 45.57522996959129102, -4.047174811376564207 ) ) ;
#8793 = B_SPLINE_CURVE_WITH_KNOTS ( 'NONE', 3,
 ( #13134, #1277, #2677, #5364, #3849, #8109, #13474, #14442, #1360, #6776, #9265, #6608, #10409, #5104, #5193, #3675, #17196, #11987, #10749, #9089, #7760, #1022, #16113, #6523, #11817, #4024, #10581, #13388, #10496, #15942, #2502, #14526, #15859, #2413, #6689, #3766, #1107, #9178, #7846, #13219, #11902, #17279, #7931, #13305, #9439, #1196, #17368, #5282, #10665, #3937, #9352, #2590, #16201, #3033, #1799, #13903, #11191, #5451, #14870, #12426, #10836, #2946, #4112, #9526, #5807, #6869, #1629, #12244, #2764, #228, #4203, #8197, #8464, #7211, #46, #9614, #16475, #13560, #1450, #137, #7128, #5544, #1539, #10927, #16387, #8551, #16295, #7047, #14964, #2854, #11016, #5633, #8288, #9789, #11102, #15049, #312, #13645, #4291, #6957, #12335, #9702, #8375, #13731, #5720, #4381, #15136, #13816, #1717, #16567, #12516, #400, #4473, #9877, #15228, #3125, #14848, #13876, #8527, #9675, #7020, #287, #9762, #16539, #1689, #10899, #202, #5517, #13790, #15025, #7186, #12488, #6930, #12575, #11164, #10989, #8436, #6841, #16358, #2918, #14938, #4265, #4353, #16270, #12217, #10812, #5608, #7104, #4085, #1604, #2741, #8171, #5423, #5779, #12308, #16175, #13534, #9501, #15107, #1424, #4446, #111, #4176, #9588, #8348, #16450, #3006, #13621, #2830, #8261, #13704, #1514, #12399, #9853, #5696, #11077, #15200, #3100, #632, #4619, #3189, #9939, #8785, #1859, #12656, #8611, #2111, #11336, #5871, #4705, #13963, #1943, #16713, #16798, #8954, #16629, #7455, #7273, #4532, #11427 ),
 .UNSPECIFIED., .F., .F.,
 ( 4, 2, 1, 2, 2, 1, 2, 2, 2, 2, 2, 2, 2, 2, 2, 2, 2, 2, 1, 2, 2, 2, 2, 2, 1, 1, 1, 2, 2, 2, 2, 1, 1, 1, 2, 2, 1, 2, 2, 2, 2, 1, 2, 2, 1, 1, 1, 2, 2, 2, 2, 2, 2, 1, 1, 1, 1, 2, 2, 2, 1, 2, 2, 2, 2, 1, 2, 2, 1, 1, 2, 2, 1, 2, 2, 1, 1, 2, 2, 2, 1, 1, 1, 2, 2, 1, 2, 2, 2, 2, 1, 2, 2, 1, 1, 2, 2, 2, 2, 2, 1, 2, 1, 2, 2, 1, 1, 2, 2, 2, 1, 2, 2, 1, 1, 2, 1, 2, 2, 4 ),
 ( 0.7109395711855112099, 0.7111682227467994721, 0.7112253856371215655, 0.7112539670822826121, 0.7112682578048631354, 0.7112825485274436588, 0.7113968743080877344, 0.7118541774306642589, 0.7127687836758173079, 0.7136833899209703569, 0.7139120414822586191, 0.7141406930435468814, 0.7145979961661234059, 0.7155126024112765659, 0.7159699055338530904, 0.7161985570951413527, 0.7162271385403022883, 0.7162557199854633350, 0.7163128828757854283, 0.7164272086564296149, 0.7173418149015825529, 0.7182564211467356019, 0.7187137242693121264, 0.7187280149918926497, 0.7187423057144731731, 0.7187708871596342197, 0.7188280500499563130, 0.7189423758306004997, 0.7191710273918888729, 0.7196283305144656195, 0.7198569820757539928, 0.7199141449660760861, 0.7199427264112371327, 0.7199570171338176561, 0.7199641624951078622, 0.7199677351757530763, 0.7199713078563981794, 0.7200856336370424771, 0.7210002398821965253, 0.7211145656628408229, 0.7212288914434851206, 0.7214575430047736049, 0.7219148461273506845, 0.7228294523725047327, 0.7232867554950818123, 0.7235154070563702966, 0.7236297328370145943, 0.7236868957273367986, 0.7237440586176588919, 0.7246586648628129401, 0.7248873164241015354, 0.7249444793144236288, 0.7249587700370041521, 0.7249730607595846754, 0.7250016422047458331, 0.7251159679853900197, 0.7255732711079670993, 0.7260305742305441790, 0.7261449000111884766, 0.7262020629015105699, 0.7262592257918326633, 0.7264878773531212586, 0.7274024835982753068, 0.7283170898434294660, 0.7285457414047180613, 0.7286600671853622480, 0.7286743579079427713, 0.7286886486305232946, 0.7287172300756844523, 0.7287743929660065456, 0.7292316960885836252, 0.7310609085788918327, 0.7311180714692140370, 0.7311466529143750837, 0.7311752343595361303, 0.7312895601401804280, 0.7315182117014689123, 0.7319755148240459919, 0.7328901210692001511, 0.7333474241917772307, 0.7335760757530658260, 0.7336332386433879194, 0.7336475293659684427, 0.7336546747272587599, 0.7336618200885489660, 0.7336904015337100127, 0.7338047273143543103, 0.7347193335595083585, 0.7356339398046622957, 0.7360912429272392643, 0.7361198243724004220, 0.7361341150949809453, 0.7361484058175614686, 0.7362055687078835620, 0.7363198944885278596, 0.7365485460498163439, 0.7370058491723933125, 0.7372345007336817968, 0.7373488265143259834, 0.7374059894046481878, 0.7374631522949702811, 0.7383777585401242183, 0.7386064101014127026, 0.7386349915465737492, 0.7386492822691542726, 0.7386635729917347959, 0.7387207358820570002, 0.7388350616627011869, 0.7392923647852781555, 0.7397496679078551240, 0.7398639936884994217, 0.7398782844110799450, 0.7398925751336604684, 0.7399211565788215150, 0.7399783194691436083, 0.7400926452497877950, 0.7401498081401099993, 0.7401783895852710460, 0.7401926803078515693, 0.7402069710304320926 ),
 .UNSPECIFIED. ) ;
#8794 = CARTESIAN_POINT ( 'NONE',  ( 8.071977012489314873, 69.87388874300927455, -10.82096426686017665 ) ) ;
#8795 = CARTESIAN_POINT ( 'NONE',  ( -12.00000000000000178, 7.213974596215562585, 3.899036354794875425 ) ) ;
#8796 = CARTESIAN_POINT ( 'NONE',  ( 12.00366664929724969, 30.65787929842621651, -6.177632669743041482 ) ) ;
#8797 = ADVANCED_FACE ( 'NONE', ( #15577 ), #10223, .T. ) ;
#8798 = CARTESIAN_POINT ( 'NONE',  ( -12.73519230341753961, 56.09167882185248288, 4.479426581004548602 ) ) ;
#8799 = CARTESIAN_POINT ( 'NONE',  ( -2.973539139891043348, 50.57300316080052482, 13.17058001520311805 ) ) ;
#8800 = CARTESIAN_POINT ( 'NONE',  ( 4.129670684472704245, 32.82848721344360854, 12.85288430302258256 ) ) ;
#8801 = CARTESIAN_POINT ( 'NONE',  ( 5.614818628722479055, 42.97613777251347500, -12.27697129638437268 ) ) ;
#8802 = CARTESIAN_POINT ( 'NONE',  ( 12.90854670894318268, 39.57182124627381370, -3.955391283021399751 ) ) ;
#8803 = ORIENTED_EDGE ( 'NONE', *, *, #12815, .T. ) ;
#8804 = CARTESIAN_POINT ( 'NONE',  ( -13.24278598375631510, 61.83745329285113002, -2.622749156585664210 ) ) ;
#8805 = EDGE_LOOP ( 'NONE', ( #15394, #7753 ) ) ;
#8806 = ORIENTED_EDGE ( 'NONE', *, *, #11694, .F. ) ;
#8807 = CARTESIAN_POINT ( 'NONE',  ( -4.171729424061791036, 29.53000000000000114, 12.83926296998457239 ) ) ;
#8808 = CARTESIAN_POINT ( 'NONE',  ( 1.561832610794586538E-12, -20.81249999999995026, -18.62500000000000000 ) ) ;
#8809 = CARTESIAN_POINT ( 'NONE',  ( 10.71586849478361536, 48.11818100869080439, 8.210984778465897804 ) ) ;
#8810 = CARTESIAN_POINT ( 'NONE',  ( 2.469740553831996976, 58.09120330256963172, -13.27217913048357723 ) ) ;
#8811 = CARTESIAN_POINT ( 'NONE',  ( 7.866550464026706102, 78.88325915401534871, -10.98022871454362281 ) ) ;
#8812 = CARTESIAN_POINT ( 'NONE',  ( -7.576616670048093940E-16, 75.67999999999999261, 12.37355403259654985 ) ) ;
#8813 = CARTESIAN_POINT ( 'NONE',  ( 10.72039879472368185, -3.110307960253515263E-15, -6.101375431309464581 ) ) ;
#8814 = MANIFOLD_SOLID_BREP ( 'Chamfer1', #11991 ) ;
#8815 = CARTESIAN_POINT ( 'NONE',  ( -9.672208996725832009, 46.56228947212231617, -9.418029512036609319 ) ) ;
#8816 = EDGE_CURVE ( 'NONE', #668, #13318, #15140, .T. ) ;
#8817 = CARTESIAN_POINT ( 'NONE',  ( 6.750022565184456980, 31.92926174983938026, 11.69132992304556495 ) ) ;
#8818 = CARTESIAN_POINT ( 'NONE',  ( -11.37500000000039790, -18.76562499999993605, 4.711679271993001628 ) ) ;
#8819 = CARTESIAN_POINT ( 'NONE',  ( 8.150611293951293135, 53.98965040082899947, 10.77109208829301323 ) ) ;
#8820 = VERTEX_POINT ( 'NONE', #16919 ) ;
#8821 = DIRECTION ( 'NONE',  ( 0.000000000000000000, -1.000000000000000000, 0.000000000000000000 ) ) ;
#8822 = ORIENTED_EDGE ( 'NONE', *, *, #5305, .F. ) ;
#8823 = AXIS2_PLACEMENT_3D ( 'NONE', #2635, #13346, #1236 ) ;
#8824 = CARTESIAN_POINT ( 'NONE',  ( 5.407998797888095233, 66.98416787033841047, -12.36956158942780704 ) ) ;
#8825 = CARTESIAN_POINT ( 'NONE',  ( -9.552639591052204498E-13, -95.73749999999976978, 11.37500000000000000 ) ) ;
#8826 = CARTESIAN_POINT ( 'NONE',  ( 1.982521523170245906E-06, 77.68005525700222336, 13.49999999999970690 ) ) ;
#8827 = CARTESIAN_POINT ( 'NONE',  ( -3.733449871309725498, 59.54576182871864631, 12.97394819335584337 ) ) ;
#8828 = CARTESIAN_POINT ( 'NONE',  ( 15.31996850146886580, 8.007813437504038845, 9.831838144771181121 ) ) ;
#8829 = DIRECTION ( 'NONE',  ( 1.000000000000000000, 8.673617379884035472E-17, 0.000000000000000000 ) ) ;
#8830 = B_SPLINE_CURVE_WITH_KNOTS ( 'NONE', 3,
 ( #4513, #8330, #3167, #8507, #9568, #5591, #2987, #11144, #12201, #6823, #93, #15088, #13856, #5498, #1498, #10880, #11233, #16608, #9921, #8418, #12469, #12557, #13603, #9743, #1760, #270, #14919, #16250, #4156, #4426, #15270, #13516, #12289, #13685, #184, #16520, #5851, #2812, #6913, #10970, #16339, #16432, #442, #13770, #1671, #4246, #5678, #7085, #9657, #15007, #7170, #1407, #1583, #4334, #354, #7002, #11058, #5761, #9835, #15180, #3082, #7519, #10261, #8854, #14122, #10008 ),
 .UNSPECIFIED., .F., .F.,
 ( 4, 2, 2, 2, 2, 2, 2, 2, 2, 2, 2, 2, 2, 2, 2, 2, 2, 2, 2, 2, 2, 2, 2, 2, 2, 2, 2, 2, 2, 2, 2, 2, 4 ),
 ( 0.000000000000000000, 0.002635407943176078672, 0.005270815886352157344, 0.006588519857940197330, 0.007906223829528238184, 0.01054163177270431989, 0.01185933574429236248, 0.01317703971588040680, 0.01581244765905649372, 0.01713015163064453630, 0.01844785560223257889, 0.01976555957382062148, 0.02108326354540866060, 0.02240096751699670319, 0.02305981950279072101, 0.02371867148858473884, 0.02404809748148175122, 0.02437752347437876013, 0.02470694946727576904, 0.02503637546017278143, 0.02536580145306978687, 0.02569522744596679925, 0.02635407943176082748, 0.02701293141755485919, 0.02767178340334888742, 0.02898948737493693695, 0.03162489531811304294, 0.03294259928970109941, 0.03426030326128915587, 0.03689571120446526187, 0.03821341517605331140, 0.03953111914764136786, 0.04216652709081747386 ),
 .UNSPECIFIED. ) ;
#8831 = CARTESIAN_POINT ( 'NONE',  ( 13.34200449954298939, 72.35767147386656006, 2.065204973313191861 ) ) ;
#8832 = CARTESIAN_POINT ( 'NONE',  ( 8.336922857196812586, 66.86199470162991076, -10.62209661523931814 ) ) ;
#8833 = CARTESIAN_POINT ( 'NONE',  ( -11.76794919243112325, 30.78000000000001180, -3.823638476888998827 ) ) ;
#8834 = CARTESIAN_POINT ( 'NONE',  ( -13.49999999999999822, 56.07999999999999119, 4.386415899144235908 ) ) ;
#8835 = CARTESIAN_POINT ( 'NONE',  ( -2.425051341520653825, 52.26719589608618577, -13.28041211626022644 ) ) ;
#8836 =( BOUNDED_CURVE ( )  B_SPLINE_CURVE ( 2, ( #6051, #16805, #4712, #2036, #730, #6138, #11517, #11604, #10458, #14317, #7717, #17065, #5063 ),
 .UNSPECIFIED., .F., .F. ) 
 B_SPLINE_CURVE_WITH_KNOTS ( ( 3, 2, 2, 2, 2, 2, 3 ),
 ( 0.4669843698996809511, 0.4698145782021032613, 0.4754749948069478260, 0.4811354114117924463, 0.4867958280166371221, 0.4924562446214816869, 0.4952864492504068794 ),
 .UNSPECIFIED. ) 
 CURVE ( )  GEOMETRIC_REPRESENTATION_ITEM ( )  RATIONAL_B_SPLINE_CURVE ( ( 0.9755282581475768211, 0.9755282581475770431, 1.000000000000000000, 0.9510565162951535312, 1.000000000000000000, 0.9510565162951535312, 1.000000000000000000, 0.9510565162951535312, 1.000000000000000000, 0.9510565162951535312, 1.000000000000000000, 0.9755282899109183337, 0.9755282581476180104 ) ) 
 REPRESENTATION_ITEM ( '' )  );
#8837 = CARTESIAN_POINT ( 'NONE',  ( -13.49999999999999822, 51.78000000000000114, -4.386415899144240349 ) ) ;
#8838 = AXIS2_PLACEMENT_3D ( 'NONE', #1349, #10485, #16018 ) ;
#8839 = CARTESIAN_POINT ( 'NONE',  ( 18.02388005911709001, 8.055054232036098938, -0.3546005442045098710 ) ) ;
#8840 = CARTESIAN_POINT ( 'NONE',  ( -6.210469887590529758, 68.45252731434959514, 11.99403323395378607 ) ) ;
#8841 = CARTESIAN_POINT ( 'NONE',  ( 1.561832610794586538E-12, -54.11249999999986926, -18.62500000000000000 ) ) ;
#8842 = EDGE_CURVE ( 'NONE', #16308, #9435, #6070, .T. ) ;
#8843 = CARTESIAN_POINT ( 'NONE',  ( 10.92172942406178926, 71.12999999999999545, 7.935100905948387684 ) ) ;
#8844 = CARTESIAN_POINT ( 'NONE',  ( -7.714727599197335195, -5.203124999999987566, -18.62500000000064304 ) ) ;
#8845 = CARTESIAN_POINT ( 'NONE',  ( -5.251609085175493519, 65.49012858565386352, 12.43669339650761607 ) ) ;
#8846 = DIRECTION ( 'NONE',  ( 0.000000000000000000, 0.000000000000000000, 1.000000000000000000 ) ) ;
#8847 = CARTESIAN_POINT ( 'NONE',  ( -13.49999999999999822, 2.779999999999990923, -4.386415899144240349 ) ) ;
#8848 = CARTESIAN_POINT ( 'NONE',  ( -8.343458848123582072, 24.38000000000000611, 11.48378591275254124 ) ) ;
#8849 = ORIENTED_EDGE ( 'NONE', *, *, #2014, .F. ) ;
#8850 = CARTESIAN_POINT ( 'NONE',  ( 13.50000000000000000, 50.42999999999999972, 1.653273178848926867E-15 ) ) ;
#8851 = VECTOR ( 'NONE', #13639, 1000.000000000000000 ) ;
#8852 = CARTESIAN_POINT ( 'NONE',  ( -12.95000749831451969, 31.79345314003229817, -3.814302809370596847 ) ) ;
#8853 = CARTESIAN_POINT ( 'NONE',  ( 9.825225734620730123, 75.07017187311475936, 9.260671064715687351 ) ) ;
#8854 = CARTESIAN_POINT ( 'NONE',  ( 11.28538604045423810, -4.913438141674765840E-17, -1.789734987990715620 ) ) ;
#8855 = DIRECTION ( 'NONE',  ( 0.7572320727871473256, 0.000000000000000000, 0.6531459162717628830 ) ) ;
#8856 = CARTESIAN_POINT ( 'NONE',  ( 2.607531440858944223E-15, 75.17999999999997840, -14.19474002721660355 ) ) ;
#8857 = CARTESIAN_POINT ( 'NONE',  ( 13.40294794219552621, 51.48823289360313282, -1.671099717773980586 ) ) ;
#8858 = CARTESIAN_POINT ( 'NONE',  ( -13.50005243685980183, 37.92238217705867953, -0.2158979556258536492 ) ) ;
#8859 = VECTOR ( 'NONE', #12110, 1000.000000000000000 ) ;
#8860 = ADVANCED_FACE ( 'NONE', ( #14952 ), #12142, .F. ) ;
#8861 = CARTESIAN_POINT ( 'NONE',  ( 11.98477050297872104, 36.65933795633807790, -6.214151509854474398 ) ) ;
#8862 = CARTESIAN_POINT ( 'NONE',  ( -4.711679271994915652, -18.69687499999997726, 11.37499999999960210 ) ) ;
#8863 = DIRECTION ( 'NONE',  ( -0.5000000000000093259, 0.000000000000000000, 0.8660254037844333785 ) ) ;
#8864 = CARTESIAN_POINT ( 'NONE',  ( -12.38439141012284139, 77.12633956890614684, 5.378321227196528831 ) ) ;
#8865 = CARTESIAN_POINT ( 'NONE',  ( 4.178864255851000829E-14, 61.67999999999999261, 13.50000000000000000 ) ) ;
#8866 = CARTESIAN_POINT ( 'NONE',  ( 3.201461801489201786, 41.79502229956779047, 13.11535449225857519 ) ) ;
#8867 = CARTESIAN_POINT ( 'NONE',  ( 13.23077815530012025, 48.52472391739948421, -2.682647111088163339 ) ) ;
#8868 = CARTESIAN_POINT ( 'NONE',  ( 3.636496289402157078, 12.03000000000001357, -11.19198476289190936 ) ) ;
#8869 = VERTEX_POINT ( 'NONE', #14690 ) ;
#8870 = CARTESIAN_POINT ( 'NONE',  ( -7.272992578804307939, 62.47999999999999687, -10.01041549318727064 ) ) ;
#8871 = CARTESIAN_POINT ( 'NONE',  ( -11.37500000000039790, -2.115624999999976996, 4.711679271993001628 ) ) ;
#8872 = CARTESIAN_POINT ( 'NONE',  ( -8.291044507619272909E-14, 57.17999999999999972, -13.50000000000000000 ) ) ;
#8873 = CARTESIAN_POINT ( 'NONE',  ( 3.636496289402157078, 30.03000000000000114, -11.19198476289190936 ) ) ;
#8874 = CYLINDRICAL_SURFACE ( 'NONE', #15843, 13.50000000000000000 ) ;
#8875 = CARTESIAN_POINT ( 'NONE',  ( 18.62499999999934985, -65.55937499999983231, 7.714727599200467800 ) ) ;
#8876 = CARTESIAN_POINT ( 'NONE',  ( 3.231997696289118593, 65.79610242286665311, 13.10760892499458308 ) ) ;
#8877 = CARTESIAN_POINT ( 'NONE',  ( -8.343458848123582072, 80.37999999999999545, 11.48378591275254124 ) ) ;
#8878 = CARTESIAN_POINT ( 'NONE',  ( -3.636496289402155746, 45.53000000000000114, 11.19198476289190936 ) ) ;
#8879 = CARTESIAN_POINT ( 'NONE',  ( -13.49458077393223832, 58.94641242465065289, 0.4787677073000579098 ) ) ;
#8880 = CARTESIAN_POINT ( 'NONE',  ( 13.35249357306756046, 45.35820753028740882, 2.049345934875174802 ) ) ;
#8881 = CARTESIAN_POINT ( 'NONE',  ( 15.58845726811991916, 0.000000000000000000, -10.99999999999996092 ) ) ;
#8882 = CARTESIAN_POINT ( 'NONE',  ( 1.486929454577674337, 80.73346438489225818, 13.41791445272210126 ) ) ;
#8883 = CARTESIAN_POINT ( 'NONE',  ( 13.07011386205427428, 30.55034935990153500, -3.379670409494439198 ) ) ;
#8884 = CARTESIAN_POINT ( 'NONE',  ( -13.46192632266902400, 55.96507060572447756, 1.013190883000425924 ) ) ;
#8885 = CARTESIAN_POINT ( 'NONE',  ( 10.92172942406178926, 53.12999999999999545, 7.935100905948387684 ) ) ;
#8886 = CARTESIAN_POINT ( 'NONE',  ( 2.742138326991311548, 64.08140283275047011, -13.21857401153399003 ) ) ;
#8887 = CARTESIAN_POINT ( 'NONE',  ( 8.375056734751542109, 9.999950376471138824, 10.58801762894534271 ) ) ;
#8888 = CARTESIAN_POINT ( 'NONE',  ( 13.03162247184152989, 39.55575396952983880, -3.525209484468003307 ) ) ;
#8889 = ORIENTED_EDGE ( 'NONE', *, *, #8131, .T. ) ;
#8890 = CARTESIAN_POINT ( 'NONE',  ( -8.595979405193384437, 61.50968794902038894, -10.42067916570242581 ) ) ;
#8891 = ORIENTED_EDGE ( 'NONE', *, *, #5478, .T. ) ;
#8892 = ORIENTED_EDGE ( 'NONE', *, *, #8420, .T. ) ;
#8893 = CARTESIAN_POINT ( 'NONE',  ( -10.92172942406178926, 28.63000000000001677, -7.935100905948389460 ) ) ;
#8894 = CARTESIAN_POINT ( 'NONE',  ( 13.16986379959834075, -31.21874999999992539, 13.16986379960055231 ) ) ;
#8895 = CARTESIAN_POINT ( 'NONE',  ( 13.06477345830753833, 48.30888743458975654, 3.400253739448160228 ) ) ;
#8896 = CARTESIAN_POINT ( 'NONE',  ( 11.47375603530613830, 57.69570350741216203, -7.113939845970555176 ) ) ;
#8897 = CARTESIAN_POINT ( 'NONE',  ( 7.201239011038929050, 78.91185591551062828, -11.41894328749275545 ) ) ;
#8898 = EDGE_CURVE ( 'NONE', #3099, #11984, #6594, .T. ) ;
#8899 = CARTESIAN_POINT ( 'NONE',  ( -11.76794919243112325, 78.07999999999999829, 3.823638476888994386 ) ) ;
#8900 = DIRECTION ( 'NONE',  ( 0.000000000000000000, 1.000000000000000000, 0.000000000000000000 ) ) ;
#8901 = CIRCLE ( 'NONE', #10029, 8.999999999999994671 ) ;
#8902 = DIRECTION ( 'NONE',  ( 0.000000000000000000, -1.000000000000000000, 0.000000000000000000 ) ) ;
#8903 = CARTESIAN_POINT ( 'NONE',  ( 8.000000000000019540, 0.000000000000000000, -24.73863375370596174 ) ) ;
#8904 = CARTESIAN_POINT ( 'NONE',  ( 11.37500000000000178, -42.69999999999988205, 9.531744055041752924E-13 ) ) ;
#8905 = CARTESIAN_POINT ( 'NONE',  ( -4.171729424061791036, 73.53000000000000114, 12.83926296998457239 ) ) ;
#8906 = CARTESIAN_POINT ( 'NONE',  ( 4.197136615133925552, 34.02912076247848461, -12.83120157241570602 ) ) ;
#8907 = ORIENTED_EDGE ( 'NONE', *, *, #3175, .T. ) ;
#8908 = CARTESIAN_POINT ( 'NONE',  ( 0.000000000000000000, 9.000000000000000000, 0.000000000000000000 ) ) ;
#8909 = ORIENTED_EDGE ( 'NONE', *, *, #8842, .T. ) ;
#8910 = CARTESIAN_POINT ( 'NONE',  ( 0.000000000000000000, 9.999999999999998224, 0.000000000000000000 ) ) ;
#8911 = CARTESIAN_POINT ( 'NONE',  ( 4.711679271994911211, -27.02187499999995524, -11.37499999999960210 ) ) ;
#8912 = CARTESIAN_POINT ( 'NONE',  ( 10.45936966163889892, 78.10386111577918200, 8.535314755708947487 ) ) ;
#8913 = CARTESIAN_POINT ( 'NONE',  ( -0.3722949396608798422, 59.66661364915144361, 13.49486841530188208 ) ) ;
#8914 = CARTESIAN_POINT ( 'NONE',  ( 15.50189495701170372, 7.815232006635826956, 10.85006967914017473 ) ) ;
#8915 = CARTESIAN_POINT ( 'NONE',  ( 12.50000000000000000, 98.93000000000002103, 1.224646799147353059E-15 ) ) ;
#8916 = CARTESIAN_POINT ( 'NONE',  ( 7.607773347999265745, 71.96560712441068119, 11.15221199550204645 ) ) ;
#8917 = CARTESIAN_POINT ( 'NONE',  ( 8.343458848123583849, 57.87999999999998835, -11.48378591275253768 ) ) ;
#8918 = CARTESIAN_POINT ( 'NONE',  ( -1.737554137020194345, 52.24245571627063356, -13.38942718112060959 ) ) ;
#8919 = CARTESIAN_POINT ( 'NONE',  ( 18.62500000000064304, -67.64062499999984368, -7.714727599197335195 ) ) ;
#8920 = CARTESIAN_POINT ( 'NONE',  ( -11.45953766701369858, 68.19652247961239766, 7.139846150206698994 ) ) ;
#8921 = CARTESIAN_POINT ( 'NONE',  ( -1.564113515457998572E-12, -12.48749999999997051, 18.62500000000000000 ) ) ;
#8922 = CARTESIAN_POINT ( 'NONE',  ( 0.000000000000000000, 9.000000000000000000, 0.000000000000000000 ) ) ;
#8923 = CARTESIAN_POINT ( 'NONE',  ( 1.561832610794586538E-12, -20.81249999999995026, -18.62500000000000000 ) ) ;
#8924 = PRODUCT_DEFINITION ( 'UNKNOWN', '', #8510, #1183 ) ;
#8925 = CARTESIAN_POINT ( 'NONE',  ( -2.195697726732460442, 65.60106443141478394, 13.32051239355739725 ) ) ;
#8926 = CARTESIAN_POINT ( 'NONE',  ( 17.32050807568873552, 0.000000000000000000, 8.000000000000085265 ) ) ;
#8927 = CARTESIAN_POINT ( 'NONE',  ( 8.992436155572725909, 8.063482198985079563, -15.58776297682138079 ) ) ;
#8928 = CARTESIAN_POINT ( 'NONE',  ( -10.92172942406178926, 26.63000000000001322, -7.935100905948389460 ) ) ;
#8929 = EDGE_LOOP ( 'NONE', ( #16993, #133, #2280, #6885 ) ) ;
#8930 = DIRECTION ( 'NONE',  ( -0.000000000000000000, -1.000000000000000000, -0.000000000000000000 ) ) ;
#8931 = AXIS2_PLACEMENT_3D ( 'NONE', #13094, #2205, #15818 ) ;
#8932 = CARTESIAN_POINT ( 'NONE',  ( -11.99429206528581737, 31.70121606863765606, -6.201385207760043095 ) ) ;
#8933 = CARTESIAN_POINT ( 'NONE',  ( 9.381058047339037032, 75.04754594223111042, 9.717309665381625550 ) ) ;
#8934 = CARTESIAN_POINT ( 'NONE',  ( 13.50001914872373909, 60.43013035372702291, -0.003958280579135459859 ) ) ;
#8935 = EDGE_CURVE ( 'NONE', #16628, #11619, #706, .T. ) ;
#8936 = CARTESIAN_POINT ( 'NONE',  ( 2.138189944381242213, 63.10311857767972299, -13.49999999999999822 ) ) ;
#8937 = CARTESIAN_POINT ( 'NONE',  ( -10.92172942406179104, 76.23000000000000398, 7.935100905948387684 ) ) ;
#8938 = CARTESIAN_POINT ( 'NONE',  ( 13.50106199340143043, 51.43115321150168739, -0.03627323424068121249 ) ) ;
#8939 = PRESENTATION_LAYER_ASSIGNMENT (  '', '', ( #15396 ) ) ;
#8940 = CARTESIAN_POINT ( 'NONE',  ( -12.98462285426537299, 38.06247337552851917, 3.704199847612075214 ) ) ;
#8941 = CARTESIAN_POINT ( 'NONE',  ( 12.65007964138050411, 36.60209030862610291, -4.758271190386921035 ) ) ;
#8942 = CARTESIAN_POINT ( 'NONE',  ( 8.043339635996298753, -38.46874999999992895, 8.043339635997652337 ) ) ;
#8943 = CARTESIAN_POINT ( 'NONE',  ( 0.000000000000000000, 0.000000000000000000, 0.000000000000000000 ) ) ;
#8944 = CARTESIAN_POINT ( 'NONE',  ( -6.376503178677815242, 77.44599626364721701, 11.89916936316262763 ) ) ;
#8945 = CARTESIAN_POINT ( 'NONE',  ( -13.49999999999999822, 61.07999999999999829, 4.386415899144235020 ) ) ;
#8946 = CARTESIAN_POINT ( 'NONE',  ( 6.484162807585885702, 41.91833735075831413, 11.84678101249536475 ) ) ;
#8947 = ORIENTED_EDGE ( 'NONE', *, *, #10230, .T. ) ;
#8948 = CARTESIAN_POINT ( 'NONE',  ( -7.272992578804307939, 15.47999999999999865, -10.01041549318726886 ) ) ;
#8949 = ORIENTED_EDGE ( 'NONE', *, *, #3945, .F. ) ;
#8950 = CARTESIAN_POINT ( 'NONE',  ( -11.76794919243112325, 59.92999999999999972, -2.882316262207890869E-15 ) ) ;
#8951 = CARTESIAN_POINT ( 'NONE',  ( -1.564113515457998370E-12, -71.83749999999979252, 18.62500000000000000 ) ) ;
#8952 = FACE_OUTER_BOUND ( 'NONE', #461, .T. ) ;
#8953 = CARTESIAN_POINT ( 'NONE',  ( 10.92172942406178926, -2.869999999999997442, 7.935100905948385908 ) ) ;
#8954 = CARTESIAN_POINT ( 'NONE',  ( -0.06471714588535149026, 43.18232697961442312, -13.49985647836149028 ) ) ;
#8955 = CARTESIAN_POINT ( 'NONE',  ( 0.8629412905205349205, 76.14897181464817777, -13.47239168749351990 ) ) ;
#8956 = VECTOR ( 'NONE', #10312, 1000.000000000000000 ) ;
#8957 = EDGE_CURVE ( 'NONE', #10808, #10491, #11315, .T. ) ;
#8958 = CARTESIAN_POINT ( 'NONE',  ( -13.16986379959834252, -89.49374999999979252, -13.16986379960055054 ) ) ;
#8959 = CARTESIAN_POINT ( 'NONE',  ( -4.171729424061791036, 77.53000000000000114, 12.83926296998457239 ) ) ;
#8960 = CARTESIAN_POINT ( 'NONE',  ( -11.76794919243112325, 53.92999999999999972, -2.882316262207890869E-15 ) ) ;
#8961 = FACE_OUTER_BOUND ( 'NONE', #130, .T. ) ;
#8962 = CARTESIAN_POINT ( 'NONE',  ( -13.47367793928326840, 58.90090033977541140, -0.8432173026106429825 ) ) ;
#8963 = CARTESIAN_POINT ( 'NONE',  ( 13.49685988162643469, 45.41999658439461030, 0.2915229779186118697 ) ) ;
#8964 = CARTESIAN_POINT ( 'NONE',  ( 13.43090557185185752, 69.38241981859624730, 1.365210260054945390 ) ) ;
#8965 = LINE ( 'NONE', #11608, #1572 ) ;
#8966 = CARTESIAN_POINT ( 'NONE',  ( 13.29842525421480914, 30.34827244870920637, 2.324384417915165812 ) ) ;
#8967 = CARTESIAN_POINT ( 'NONE',  ( -12.94454544090478976, 56.06735303853458419, 3.835177592674254843 ) ) ;
#8968 = CARTESIAN_POINT ( 'NONE',  ( -8.647676296952441888, 50.34754238603772336, 10.36673610620846375 ) ) ;
#8969 = CARTESIAN_POINT ( 'NONE',  ( 0.5905603839040489689, 64.15876562730046828, -13.50000000000000000 ) ) ;
#8970 = DIRECTION ( 'NONE',  ( 0.000000000000000000, 0.000000000000000000, 1.000000000000000000 ) ) ;
#8971 = CARTESIAN_POINT ( 'NONE',  ( 13.45524155940220368, 39.46821381739253809, -1.102643116948291313 ) ) ;
#8972 = ORIENTED_EDGE ( 'NONE', *, *, #10059, .F. ) ;
#8973 = CARTESIAN_POINT ( 'NONE',  ( -4.862930340901737480, 61.35534921865077251, -12.59544805092636999 ) ) ;
#8974 = CARTESIAN_POINT ( 'NONE',  ( 9.520470885617715595, 5.129999999999995453, 6.917026985038135400 ) ) ;
#8975 = VERTEX_POINT ( 'NONE', #7898 ) ;
#8976 = ORIENTED_EDGE ( 'NONE', *, *, #15443, .F. ) ;
#8977 = CARTESIAN_POINT ( 'NONE',  ( 10.92172942406179104, 27.73000000000000398, -7.935100905948385908 ) ) ;
#8978 = CARTESIAN_POINT ( 'NONE',  ( 18.62499999999935341, -106.1093749999997868, 7.714727599200469577 ) ) ;
#8979 = CARTESIAN_POINT ( 'NONE',  ( 6.668950942393352399, 47.92593842342445498, 11.73779662346200503 ) ) ;
#8980 = EDGE_CURVE ( 'NONE', #546, #1713, #1162, .T. ) ;
#8981 = CARTESIAN_POINT ( 'NONE',  ( 4.566661204442511668, 58.01567420843213796, -12.70452432719981672 ) ) ;
#8982 = CARTESIAN_POINT ( 'NONE',  ( 2.592248576106782831, 79.08679227953400925, -13.24881110508173698 ) ) ;
#8983 = CARTESIAN_POINT ( 'NONE',  ( -7.272992578804307939, 83.47999999999998977, -10.01041549318726886 ) ) ;
#8984 = CARTESIAN_POINT ( 'NONE',  ( 2.138192755968095327, 0.7568815234145580551, 13.49999908646005231 ) ) ;
#8985 = CARTESIAN_POINT ( 'NONE',  ( 4.171729424061789260, 40.82999999999999829, 12.83926296998457417 ) ) ;
#8986 = DIRECTION ( 'NONE',  ( -0.000000000000000000, -1.000000000000000000, -0.000000000000000000 ) ) ;
#8987 = CARTESIAN_POINT ( 'NONE',  ( 9.538709233711902776E-13, -13.56249999999995026, -11.37500000000000178 ) ) ;
#8988 = CARTESIAN_POINT ( 'NONE',  ( 12.50000000000000000, 98.93000000000002103, -8.999999999999996447 ) ) ;
#8989 = CARTESIAN_POINT ( 'NONE',  ( 2.927080096553553279, 34.07475512125041206, -13.17907647301958285 ) ) ;
#8990 = ORIENTED_EDGE ( 'NONE', *, *, #10879, .T. ) ;
#8991 = CARTESIAN_POINT ( 'NONE',  ( 0.000000000000000000, 80.93000000000000682, -13.50000000000000000 ) ) ;
#8992 = ORIENTED_EDGE ( 'NONE', *, *, #139, .T. ) ;
#8993 = CARTESIAN_POINT ( 'NONE',  ( -10.92172942406179104, 17.22999999999999687, 7.935100905948385908 ) ) ;
#8994 = CARTESIAN_POINT ( 'NONE',  ( 11.37500000000000000, -83.24999999999980105, 9.531744055041752924E-13 ) ) ;
#8995 = CARTESIAN_POINT ( 'NONE',  ( 6.742658785962751367, 77.92880199888011816, 11.70377657027630747 ) ) ;
#8996 = CARTESIAN_POINT ( 'NONE',  ( -0.4161179423075612727, 59.66503801145354657, 13.49364511791329058 ) ) ;
#8997 = FACE_OUTER_BOUND ( 'NONE', #5511, .T. ) ;
#8998 = CARTESIAN_POINT ( 'NONE',  ( 0.000000000000000000, 73.00000000000001421, 0.000000000000000000 ) ) ;
#8999 = CARTESIAN_POINT ( 'NONE',  ( 13.50000000000000355, 48.57999999999999829, -4.386415899144233244 ) ) ;
#9000 = CARTESIAN_POINT ( 'NONE',  ( -11.39744115779548395, 71.20036747441211844, 7.238542865686949490 ) ) ;
#9001 = DIRECTION ( 'NONE',  ( 0.000000000000000000, -1.000000000000000000, 0.000000000000000000 ) ) ;
#9002 = B_SPLINE_CURVE_WITH_KNOTS ( 'NONE', 3,
 ( #689, #11064, #10081, #14024 ),
 .UNSPECIFIED., .F., .F.,
 ( 4, 4 ),
 ( 2.376698214958262694E-07, 0.007646667280170315988 ),
 .UNSPECIFIED. ) ;
#9003 = CARTESIAN_POINT ( 'NONE',  ( -18.62500000000000000, -74.92499999999982663, -1.562973063126292555E-12 ) ) ;
#9004 = CARTESIAN_POINT ( 'NONE',  ( 1.442968444427624064, 68.73190990305209880, 13.42312217546540687 ) ) ;
#9005 = CARTESIAN_POINT ( 'NONE',  ( -18.62499999999934985, -40.58437499999990905, -7.714727599200458918 ) ) ;
#9006 = CARTESIAN_POINT ( 'NONE',  ( 6.247472632322534913, 54.95119552819922859, -11.96753039951391884 ) ) ;
#9007 = TOROIDAL_SURFACE ( 'NONE', #1362, 6.000000000000001776, 6.000000000000000000 ) ;
#9008 = CARTESIAN_POINT ( 'NONE',  ( 18.62500000000000000, -33.29999999999991900, 1.560692158462880521E-12 ) ) ;
#9009 = CARTESIAN_POINT ( 'NONE',  ( -9.792966264564828549, 65.29152017548152287, 9.292365692678918876 ) ) ;
#9010 = LINE ( 'NONE', #8926, #7347 ) ;
#9011 = CARTESIAN_POINT ( 'NONE',  ( -1.471159980561823621, 35.62713808519091430, 13.41980265001063088 ) ) ;
#9012 = EDGE_LOOP ( 'NONE', ( #12130, #5818, #10531, #16006, #10387, #16708, #2410, #12595, #6497, #6602, #8892, #3619, #4440, #14328, #5718, #3601, #12763, #3136, #14781, #6555, #10129, #9414, #9083, #9787, #13194, #13363, #9410, #5865, #3367, #14090, #8891, #12740, #15497, #13912, #2052, #14075, #2762, #653, #5691, #15959, #13617, #3952, #12953, #11448, #3670, #2736, #9175, #5422, #3847, #11766, #7206 ) ) ;
#9013 = CYLINDRICAL_SURFACE ( 'NONE', #10691, 26.00000000000000355 ) ;
#9014 = CARTESIAN_POINT ( 'NONE',  ( -5.388417691150885425, 40.37512624867186872, -12.37871880772484801 ) ) ;
#9015 = CARTESIAN_POINT ( 'NONE',  ( -11.82702148097626882, 31.68881418104456316, -6.509358658607543369 ) ) ;
#9016 = CIRCLE ( 'NONE', #2771, 26.00000000000000355 ) ;
#9017 = CARTESIAN_POINT ( 'NONE',  ( 0.000000000000000000, 9.000000000000000000, 0.000000000000000000 ) ) ;
#9018 = CARTESIAN_POINT ( 'NONE',  ( 10.62943871048521416, 60.11330761422155433, 8.322610308588142658 ) ) ;
#9019 = B_SPLINE_CURVE_WITH_KNOTS ( 'NONE', 3,
 ( #712, #16965, #2276, #7797, #3530, #14387, #7617, #6123, #12994, #4956, #11502, #16878, #10359, #4783, #10185, #876, #965, #3617, #7703, #17137, #11851, #15804, #3708, #9126, #14475, #2363, #16146, #15890, #9383, #12019, #14649, #10697, #14907, #3971, #3881, #4144, #5485, #6722, #16236, #16064, #10528, #4055, #5226, #2537, #10867, #9299, #7877, #7965, #14818, #2801, #14733, #9469, #10611, #12278, #2621, #1308, #3799, #9211, #12100, #14562, #2447, #13254, #2711, #13336, #17482, #8054, #13419, #1141, #6552, #5397, #1489, #15978, #8140, #11932, #10781, #17398, #1227, #13505, #8232, #1395, #17312, #9557, #6639, #5137, #5314, #6811, #12189, #81, #13593, #6904, #3248, #7337, #9733, #16598, #4237, #8322, #16685, #11049, #15259, #16421, #1574, #16510, #8672 ),
 .UNSPECIFIED., .F., .F.,
 ( 4, 2, 2, 1, 2, 2, 2, 2, 2, 2, 2, 2, 2, 1, 2, 2, 2, 2, 2, 2, 2, 1, 2, 2, 2, 2, 2, 2, 2, 2, 2, 2, 2, 2, 2, 2, 2, 2, 2, 2, 2, 2, 2, 2, 2, 1, 2, 1, 2, 2, 1, 1, 2, 2, 4 ),
 ( 0.004923257755196806459, 0.005842365896827374054, 0.006072142932235015736, 0.006301919967642657418, 0.006761474038457940781, 0.007680582180088505774, 0.007795470697792326181, 0.007910359215496145721, 0.008140136250903783066, 0.008599690321719061226, 0.009518798463349617545, 0.009748575498757256624, 0.009863464016461077899, 0.009978352534164899174, 0.01043790660498018601, 0.01135701474661075794, 0.01181656881742604304, 0.01227612288824132813, 0.01319523102987190180, 0.01365478510068719037, 0.01376967361839101164, 0.01388456213609483118, 0.01411433917150247894, 0.01503344731313306475, 0.01549300138394835852, 0.01560788990165218500, 0.01572277841935600801, 0.01595255545476365749, 0.01687166359639424851, 0.01779077173802484646, 0.01870987987965544094, 0.01916943395047073992, 0.01962898802128603543, 0.02146720430454722439, 0.02192675837536253031, 0.02238631244617782234, 0.02330542058780842030, 0.02376497465862371927, 0.02422452872943901131, 0.02514363687106960232, 0.02606274501270019334, 0.02698185315433078435, 0.02882006943759196638, 0.02927962350840725841, 0.02950940054381490790, 0.02973917757922255739, 0.03065828572085315534, 0.03111783979166844738, 0.03123272830937227212, 0.03126145043879823004, 0.03129017256822418797, 0.03134761682707610381, 0.03157739386248376023, 0.03249650200411437900, 0.03433471828737562348 ),
 .UNSPECIFIED. ) ;
#9020 = CARTESIAN_POINT ( 'NONE',  ( -4.171729424061791036, 3.530000000000005578, 12.83926296998457239 ) ) ;
#9021 = CARTESIAN_POINT ( 'NONE',  ( -9.922634972987312452, 53.28481884420132531, 9.153759857451145621 ) ) ;
#9022 = CARTESIAN_POINT ( 'NONE',  ( 9.520470885617717371, 55.73000000000000398, -6.917026985038131848 ) ) ;
#9023 = CARTESIAN_POINT ( 'NONE',  ( 0.000000000000000000, 0.000000000000000000, 0.000000000000000000 ) ) ;
#9024 = CARTESIAN_POINT ( 'NONE',  ( 13.50000000000000355, 71.58000000000001251, -4.386415899144233244 ) ) ;
#9025 = CARTESIAN_POINT ( 'NONE',  ( 11.71290578796123150, 51.67940127277162077, -6.712522446964136691 ) ) ;
#9026 = CARTESIAN_POINT ( 'NONE',  ( -13.49476779773840640, 37.91485606517741758, -0.4350515032986518316 ) ) ;
#9027 = CARTESIAN_POINT ( 'NONE',  ( 13.48567759012120959, 36.45142198522849952, -0.6217841871730820369 ) ) ;
#9028 = CARTESIAN_POINT ( 'NONE',  ( -11.37500000000039613, -16.61562499999998010, 4.711679271993000739 ) ) ;
#9029 = EDGE_CURVE ( 'NONE', #14499, #10678, #1242, .T. ) ;
#9030 = CARTESIAN_POINT ( 'NONE',  ( -6.083868223356676097, 74.45772641535832292, 12.05141389497554449 ) ) ;
#9031 = B_SPLINE_CURVE_WITH_KNOTS ( 'NONE', 3,
 ( #12554, #16429, #9741, #14036, #3350, #8765, #4424, #440, #9833, #3257, #15441, #2985, #15086, #8416, #15178, #4687, #6023, #7253, #16778, #11231, #11056, #16692, #5758, #8505, #11407, #7434, #14120, #13942, #1838, #2008, #16606, #4599, #11142, #12639, #10090, #13767, #13854, #1669, #7083, #8677, #12467, #351, #10006, #1758, #7168, #5849, #16518, #1924, #12813, #5676, #9918, #3165, #8591, #12726, #612, #525, #5934, #11314, #10514, #17037, #11492, #9109, #9197, #784, #2261, #952, #2176, #4771, #14291, #6451, #4942, #17124, #15789, #3696, #11578, #11835, #6364, #7688, #2350, #2433, #10430, #14548, #7602, #14461, #7782, #4855, #17212, #7865, #3518, #13154, #1040, #10343, #3783, #13067, #701, #5123, #3605, #5030, #15610, #15877, #6273, #6111, #16866, #14206, #10258, #11747, #10176, #15526, #3436, #8852, #2090, #7517, #12897, #6191, #16953, #8932, #12980, #863, #11661, #15697, #9015, #14373, #2874, #13577, #16128, #12174, #10681, #14891, #1292, #12260, #9283, #6623, #13491, #5299, #16047, #156, #3954, #12002, #5562, #8036, #9367, #1212, #6539, #10945, #16311, #4218, #8124, #7949, #12084, #9632, #5470, #2695, #17467, #14981, #11919, #14635, #14717, #10766, #6888, #5210, #10600, #17384, #10851, #13239, #15963, #17297, #3868, #2605, #1127, #1469, #14802, #2521, #6707, #13320, #13404, #5380, #65, #4039, #9454, #1379, #6796 ),
 .UNSPECIFIED., .F., .F.,
 ( 4, 2, 1, 1, 2, 2, 2, 2, 2, 2, 1, 2, 2, 2, 2, 2, 1, 2, 2, 1, 2, 2, 1, 1, 1, 2, 2, 2, 2, 2, 1, 2, 2, 1, 1, 1, 2, 2, 2, 2, 2, 2, 1, 1, 2, 2, 2, 2, 1, 1, 2, 2, 2, 2, 2, 1, 2, 2, 2, 2, 2, 2, 2, 2, 2, 2, 2, 1, 2, 2, 1, 1, 2, 2, 1, 2, 2, 2, 2, 2, 2, 2, 2, 1, 1, 2, 2, 2, 1, 1, 2, 2, 1, 2, 2, 2, 1, 2, 1, 1, 2, 2, 2, 2, 4 ),
 ( 0.9460866550216218140, 0.9470057531069978607, 0.9471206403676698526, 0.9471780839980058486, 0.9472068058131738466, 0.9472355276283418446, 0.9474653021496858285, 0.9479248511923739073, 0.9488439492777499540, 0.9490737237990939379, 0.9491886110597659298, 0.9492460546901019258, 0.9493034983204379218, 0.9497630473631260006, 0.9506821454485020473, 0.9511416944911900151, 0.9512565817518620070, 0.9512853035670300050, 0.9513140253821980030, 0.9513714690125339990, 0.9516012435338779829, 0.9525203416192540296, 0.9529798906619421084, 0.9532096651832860923, 0.9532671088136220883, 0.9532958306287900863, 0.9533245524439580842, 0.9534394397046300762, 0.9543585377900056788, 0.9552776358753812813, 0.9553350795057172773, 0.9553422599595092768, 0.9553494404133011653, 0.9553638013208851643, 0.9553925231360531622, 0.9555074103967251542, 0.9557371849180691381, 0.9561967339607569949, 0.9571158320461327085, 0.9573456065674765814, 0.9573743283826445793, 0.9573886892902285783, 0.9574030501978125773, 0.9574604938281485733, 0.9575753810888205653, 0.9580349301315084221, 0.9589540282168842467, 0.9591838027382282306, 0.9592986899989002225, 0.9593561336292362185, 0.9593848554444042165, 0.9594135772595722145, 0.9598731263022600713, 0.9607922243876357848, 0.9612517734303236416, 0.9613666606909956336, 0.9614241043213316296, 0.9614815479516676255, 0.9617113224730114984, 0.9626304205583873230, 0.9630899696010751798, 0.9633197441224191637, 0.9634346313830910447, 0.9634920750134270406, 0.9635495186437630366, 0.9644686167291388612, 0.9653877148145145748, 0.9654451584448505708, 0.9654738802600185688, 0.9655026020751865667, 0.9656174893358585587, 0.9658472638572024316, 0.9663068128998903994, 0.9672259109852661130, 0.9674556855066100969, 0.9675131291369460929, 0.9675705727672820888, 0.9676854600279539698, 0.9681450090706418266, 0.9690641071560175401, 0.9695236561987053969, 0.9695523780138733949, 0.9695810998290413929, 0.9696385434593773889, 0.9697534307200493808, 0.9699832052413933647, 0.9709023033267691893, 0.9713618523694570461, 0.9714767396301290381, 0.9715341832604650341, 0.9715629050756330320, 0.9715916268908010300, 0.9718214014121450139, 0.9722809504548328707, 0.9725107249761768546, 0.9726256122368487356, 0.9727404994975207275, 0.9732000485402085843, 0.9734298230615525682, 0.9735447103222245602, 0.9736021539525605561, 0.9736595975828965521, 0.9745786956682722657, 0.9750382447109602335, 0.9754977937536480903 ),
 .UNSPECIFIED. ) ;
#9032 = CARTESIAN_POINT ( 'NONE',  ( -10.68563015858318010, 77.24352929578411420, 8.250311360857775611 ) ) ;
#9033 = CARTESIAN_POINT ( 'NONE',  ( 1.321426517745528884, 62.72752481348654641, 13.43884102842175565 ) ) ;
#9034 = CARTESIAN_POINT ( 'NONE',  ( 7.500000000000000888, 105.5999945338998316, -8.557281619885975132 ) ) ;
#9035 = ORIENTED_EDGE ( 'NONE', *, *, #12229, .T. ) ;
#9036 = AXIS2_PLACEMENT_3D ( 'NONE', #5928, #6992, #5580 ) ;
#9037 = CARTESIAN_POINT ( 'NONE',  ( 3.636496289402154414, 10.83000000000000540, 11.19198476289190758 ) ) ;
#9038 = ORIENTED_EDGE ( 'NONE', *, *, #16246, .T. ) ;
#9039 = CARTESIAN_POINT ( 'NONE',  ( -9.520470885617715595, 56.63000000000000256, -6.917026985038136289 ) ) ;
#9040 = CARTESIAN_POINT ( 'NONE',  ( -8.043339635996304082, -48.94374999999985931, -8.043339635997652337 ) ) ;
#9041 = CARTESIAN_POINT ( 'NONE',  ( 8.000000000000023093, 7.773118517290098062, -17.32050807568876394 ) ) ;
#9042 = CARTESIAN_POINT ( 'NONE',  ( -13.49999999999999822, 1.780000000000000693, -4.386415899144240349 ) ) ;
#9043 = CARTESIAN_POINT ( 'NONE',  ( 13.04935142376444190, 75.55330351446269788, -3.459312735805662786 ) ) ;
#9044 = CARTESIAN_POINT ( 'NONE',  ( -13.16986379960055231, -77.00624999999982379, 13.16986379959834252 ) ) ;
#9045 = CARTESIAN_POINT ( 'NONE',  ( 2.983352907350662608, 65.78734330260596153, 13.16637178637216188 ) ) ;
#9046 = CARTESIAN_POINT ( 'NONE',  ( -8.343458848123576743, 73.47999999999998977, -11.48378591275254301 ) ) ;
#9047 = CARTESIAN_POINT ( 'NONE',  ( -9.520470885617715595, 47.62999999999999545, -6.917026985038136289 ) ) ;
#9048 = CARTESIAN_POINT ( 'NONE',  ( 17.32050807568873552, 0.000000000000000000, 8.000000000000085265 ) ) ;
#9049 = CARTESIAN_POINT ( 'NONE',  ( -13.47567420470207367, 58.95825367557104357, 0.8183608827415700393 ) ) ;
#9050 = CARTESIAN_POINT ( 'NONE',  ( 11.46240780194647613, 45.16347604483497946, 7.131845818427484218 ) ) ;
#9051 = CARTESIAN_POINT ( 'NONE',  ( 12.81028693375460925, 69.27666315554829168, 4.259893263560612375 ) ) ;
#9052 = CARTESIAN_POINT ( 'NONE',  ( 1.732537601945078443, 80.74229332225066003, 13.38860820060650347 ) ) ;
#9053 = CARTESIAN_POINT ( 'NONE',  ( 13.27581331548750398, 30.34371935371627771, 2.450248975568062093 ) ) ;
#9054 = CARTESIAN_POINT ( 'NONE',  ( -7.369715979180460508, 55.45532736720758038, -11.31094860067307550 ) ) ;
#9055 = EDGE_CURVE ( 'NONE', #4638, #2220, #13244, .T. ) ;
#9056 = CARTESIAN_POINT ( 'NONE',  ( -12.54398616578646930, 50.11135895507305094, 4.993044113767551195 ) ) ;
#9057 = CARTESIAN_POINT ( 'NONE',  ( 6.774078098304966211, 63.93013539151233715, -11.69604546737801876 ) ) ;
#9058 = CARTESIAN_POINT ( 'NONE',  ( 2.222800136090958073E-15, 0.04602540378443767399, -12.00000000000000000 ) ) ;
#9059 = CARTESIAN_POINT ( 'NONE',  ( 13.30714225929327377, 39.35008739665155986, 2.274010068040550614 ) ) ;
#9060 = ORIENTED_EDGE ( 'NONE', *, *, #6355, .F. ) ;
#9061 = CARTESIAN_POINT ( 'NONE',  ( -10.69487954465043877, 70.61620775606867539, -8.249985653213133929 ) ) ;
#9062 = CARTESIAN_POINT ( 'NONE',  ( -10.08509511462296615, 61.58369563808273028, -8.974460719705570355 ) ) ;
#9063 = CARTESIAN_POINT ( 'NONE',  ( -3.636496289402156190, 4.530000000000006466, 11.19198476289190758 ) ) ;
#9064 = ORIENTED_EDGE ( 'NONE', *, *, #2992, .T. ) ;
#9065 = CARTESIAN_POINT ( 'NONE',  ( -11.00449575567194849, 40.63425626336776020, -7.832253106132067266 ) ) ;
#9066 = EDGE_LOOP ( 'NONE', ( #3864, #16044, #13985, #7513 ) ) ;
#9067 = CARTESIAN_POINT ( 'NONE',  ( 10.92172942406178926, 27.13000000000001677, 7.935100905948385908 ) ) ;
#9068 = CARTESIAN_POINT ( 'NONE',  ( 18.62500000000000000, -107.1499999999997783, 1.560692158462880521E-12 ) ) ;
#9069 = CARTESIAN_POINT ( 'NONE',  ( 1.281689085039503961, 47.72602004897316874, 13.44796667457771377 ) ) ;
#9070 = CARTESIAN_POINT ( 'NONE',  ( 2.374394324664103717, 58.09462585364141063, -13.28956834044282331 ) ) ;
#9071 = CARTESIAN_POINT ( 'NONE',  ( 12.19260015540604769, 78.64272030694958460, -5.795731624687062045 ) ) ;
#9072 = CARTESIAN_POINT ( 'NONE',  ( 3.636496289402157078, 74.03000000000000114, -11.19198476289190936 ) ) ;
#9073 = CARTESIAN_POINT ( 'NONE',  ( -13.49999999999999822, 37.07999999999999119, 4.386415899144235908 ) ) ;
#9074 = CARTESIAN_POINT ( 'NONE',  ( 12.54984920316064922, 1.934905186679871999E-15, -1.651895503087821737 ) ) ;
#9075 = CARTESIAN_POINT ( 'NONE',  ( 10.92172942406178926, 1.129999999999992122, 7.935100905948385908 ) ) ;
#9076 = CARTESIAN_POINT ( 'NONE',  ( 7.205550358426942026, -99.99999999999997158, 10.23940715599030327 ) ) ;
#9077 = CARTESIAN_POINT ( 'NONE',  ( -8.343458848123578520, 75.48000000000000398, -11.48378591275254124 ) ) ;
#9078 = CARTESIAN_POINT ( 'NONE',  ( 9.538709233711902776E-13, -63.51249999999981810, -11.37500000000000178 ) ) ;
#9079 = ADVANCED_FACE ( 'NONE', ( #14926 ), #2730, .T. ) ;
#9080 = CARTESIAN_POINT ( 'NONE',  ( 7.499999999999998224, 108.9300000000000068, -9.367496997597600128 ) ) ;
#9081 = CARTESIAN_POINT ( 'NONE',  ( 4.272114809023935145, 34.02640058480978524, -12.80647630758542022 ) ) ;
#9082 = CARTESIAN_POINT ( 'NONE',  ( -13.34776453198840152, 73.85917255742896259, -2.021718343860550604 ) ) ;
#9083 = ORIENTED_EDGE ( 'NONE', *, *, #10587, .T. ) ;
#9084 = ORIENTED_EDGE ( 'NONE', *, *, #16917, .T. ) ;
#9085 = CARTESIAN_POINT ( 'NONE',  ( 0.000000000000000000, 0.000000000000000000, 0.000000000000000000 ) ) ;
#9086 = VERTEX_POINT ( 'NONE', #14752 ) ;
#9087 = CARTESIAN_POINT ( 'NONE',  ( 4.171729424061789260, 17.83000000000001251, 12.83926296998457239 ) ) ;
#9088 = CARTESIAN_POINT ( 'NONE',  ( 11.37500000000039613, -8.290625000000000355, -4.711679271993002516 ) ) ;
#9089 = CARTESIAN_POINT ( 'NONE',  ( -4.441115907745108338, 44.52024772551524023, 12.74888276553507538 ) ) ;
#9090 = CARTESIAN_POINT ( 'NONE',  ( -7.684034168813939303, 59.39112170478899344, 11.10103013205298872 ) ) ;
#9091 = FACE_OUTER_BOUND ( 'NONE', #9012, .T. ) ;
#9092 = CARTESIAN_POINT ( 'NONE',  ( 2.785879211291982797E-06, 6.680077384874748780, 13.49999999999942979 ) ) ;
#9093 = CARTESIAN_POINT ( 'NONE',  ( 7.771422898618976838, 66.88723588304965517, -11.03881805963236573 ) ) ;
#9094 =( BOUNDED_CURVE ( )  B_SPLINE_CURVE ( 2, ( #7025, #11081, #4535, #12660, #8614, #12492, #4450, #13966, #3010, #7189, #16455, #10905, #466, #5874, #16274, #15291, #3193, #1863, #7277, #4180, #9592, #2834, #8265, #1518, #3283, #14314, #10028, #10196, #2285, #6047, #16977, #16716, #15549, #12838, #15464, #11513, #15723, #4795, #4622, #15376, #11685, #11429, #7542, #6214, #7457, #8699, #2032, #17061, #3461, #4879, #4965, #14060, #12920, #1945, #7367, #725, #10369, #11601, #4708, #10111, #2201, #13091, #6299, #8875, #10282, #3374, #7627, #16890, #3630, #12747, #16800, #15633, #8787, #14144, #9044, #6134, #14229, #14396, #2114, #803, #13004, #634, #7713, #5959, #11339, #3542, #8958, #887, #10708, #8151, #15988, #5323, #17148, #6564, #14485, #10539, #3892 ),
 .UNSPECIFIED., .F., .F. ) 
 B_SPLINE_CURVE_WITH_KNOTS ( ( 3, 2, 2, 2, 2, 2, 2, 2, 2, 2, 2, 2, 2, 2, 2, 2, 2, 2, 2, 2, 2, 2, 2, 2, 2, 2, 2, 2, 2, 2, 2, 2, 2, 2, 2, 2, 2, 2, 2, 2, 2, 2, 2, 2, 2, 2, 2, 2, 3 ),
 ( 0.000000000000000000, 0.02083333333333333218, 0.04166666666666666435, 0.06250000000000000000, 0.08333333333333332871, 0.1041666666666666713, 0.1250000000000000000, 0.1458333333333333426, 0.1666666666666666574, 0.1875000000000000000, 0.2083333333333333426, 0.2291666666666666574, 0.2500000000000000000, 0.2708333333333333148, 0.2916666666666666852, 0.3125000000000000000, 0.3333333333333333148, 0.3541666666666666852, 0.3750000000000000000, 0.3958333333333333148, 0.4166666666666666852, 0.4375000000000000000, 0.4583333333333333148, 0.4791666666666666852, 0.5000000000000000000, 0.5208333333333333703, 0.5416666666666666297, 0.5625000000000000000, 0.5833333333333333703, 0.6041666666666666297, 0.6250000000000000000, 0.6458333333333333703, 0.6666666666666666297, 0.6875000000000000000, 0.7083333333333333703, 0.7291666666666666297, 0.7500000000000000000, 0.7708333333333333703, 0.7916666666666666297, 0.8125000000000000000, 0.8333333333333333703, 0.8541666666666666297, 0.8750000000000000000, 0.8958333333333333703, 0.9166666666666666297, 0.9375000000000000000, 0.9583333333333333703, 0.9791666666666666297, 1.000000000000000000 ),
 .UNSPECIFIED. ) 
 CURVE ( )  GEOMETRIC_REPRESENTATION_ITEM ( )  RATIONAL_B_SPLINE_CURVE ( ( 1.000000000000000000, 0.9238795325112867385, 1.000000000000000000, 0.9238795325112867385, 1.000000000000000000, 0.9238795325112867385, 1.000000000000000000, 0.9238795325112867385, 1.000000000000000000, 0.9238795325112867385, 1.000000000000000000, 0.9238795325112867385, 1.000000000000000000, 0.9238795325112867385, 1.000000000000000000, 0.9238795325112867385, 1.000000000000000000, 0.9238795325112867385, 1.000000000000000000, 0.9238795325112867385, 1.000000000000000000, 0.9238795325112867385, 1.000000000000000000, 0.9238795325112867385, 1.000000000000000000, 0.9238795325112867385, 1.000000000000000000, 0.9238795325112867385, 1.000000000000000000, 0.9238795325112867385, 1.000000000000000000, 0.9238795325112867385, 1.000000000000000000, 0.9238795325112867385, 1.000000000000000000, 0.9238795325112867385, 1.000000000000000000, 0.9238795325112867385, 1.000000000000000000, 0.9238795325112867385, 1.000000000000000000, 0.9238795325112867385, 1.000000000000000000, 0.9238795325112867385, 1.000000000000000000, 0.9238795325112867385, 1.000000000000000000, 0.9238795325112867385, 1.000000000000000000, 0.9238795325112867385, 1.000000000000000000, 0.9238795325112867385, 1.000000000000000000, 0.9238795325112867385, 1.000000000000000000, 0.9238795325112867385, 1.000000000000000000, 0.9238795325112867385, 1.000000000000000000, 0.9238795325112867385, 1.000000000000000000, 0.9238795325112867385, 1.000000000000000000, 0.9238795325112867385, 1.000000000000000000, 0.9238795325112867385, 1.000000000000000000, 0.9238795325112867385, 1.000000000000000000, 0.9238795325112867385, 1.000000000000000000, 0.9238795325112867385, 1.000000000000000000, 0.9238795325112867385, 1.000000000000000000, 0.9238795325112867385, 1.000000000000000000, 0.9238795325112867385, 1.000000000000000000, 0.9238795325112867385, 1.000000000000000000, 0.9238795325112867385, 1.000000000000000000, 0.9238795325112867385, 1.000000000000000000, 0.9238795325112867385, 1.000000000000000000, 0.9238795325112867385, 1.000000000000000000, 0.9238795325112867385, 1.000000000000000000, 0.9238795325112867385, 1.000000000000000000, 0.9238795325112867385, 1.000000000000000000, 0.9238795325112867385, 1.000000000000000000 ) ) 
 REPRESENTATION_ITEM ( '' )  );
#9095 = CARTESIAN_POINT ( 'NONE',  ( 8.343458848123578520, 53.97999999999998977, 11.48378591275254124 ) ) ;
#9096 = CARTESIAN_POINT ( 'NONE',  ( -8.147096294993618315, 71.37051073404745694, 10.76453482734664391 ) ) ;
#9097 = CARTESIAN_POINT ( 'NONE',  ( -7.714727599200467800, -94.69687499999979252, 18.62499999999934630 ) ) ;
#9098 = CARTESIAN_POINT ( 'NONE',  ( -8.053875534609741038, 68.37512698675379852, 10.85470679754551071 ) ) ;
#9099 = CARTESIAN_POINT ( 'NONE',  ( -18.62500000000000000, -74.92499999999982663, -1.562973063126292555E-12 ) ) ;
#9100 = VECTOR ( 'NONE', #5872, 1000.000000000000000 ) ;
#9101 = CARTESIAN_POINT ( 'NONE',  ( 5.720610333239705803, 54.97207370978246388, -12.22862423939397658 ) ) ;
#9102 = CARTESIAN_POINT ( 'NONE',  ( 18.62500000000000000, -16.64999999999995950, 1.560692158462880521E-12 ) ) ;
#9103 = CARTESIAN_POINT ( 'NONE',  ( -11.34091630496454073, 65.20426177971908999, 7.324935009242633299 ) ) ;
#9104 = CARTESIAN_POINT ( 'NONE',  ( 6.750022862106053623, 29.92926176209967437, 11.69132975161703669 ) ) ;
#9105 = CARTESIAN_POINT ( 'NONE',  ( -6.978456841825852131, 35.42124363644111895, 11.55651345503810923 ) ) ;
#9106 = ORIENTED_EDGE ( 'NONE', *, *, #482, .T. ) ;
#9107 = CARTESIAN_POINT ( 'NONE',  ( 11.76794919243112680, 31.57999999999999119, -3.823638476888993942 ) ) ;
#9108 = CARTESIAN_POINT ( 'NONE',  ( 0.000000000000000000, 80.93000000000000682, 0.000000000000000000 ) ) ;
#9109 = CARTESIAN_POINT ( 'NONE',  ( -11.62183027776853628, 32.18583764462453445, 6.871631281967373717 ) ) ;
#9110 = CARTESIAN_POINT ( 'NONE',  ( 0.4719270757883078371, 73.16303128037343129, -13.49180536696172616 ) ) ;
#9111 = CARTESIAN_POINT ( 'NONE',  ( 8.915328836987622907, 60.02504728364877451, 10.14169724999834621 ) ) ;
#9112 = CARTESIAN_POINT ( 'NONE',  ( -13.49999999999999822, -2.920000000000003926, 4.386415899144235908 ) ) ;
#9113 = CARTESIAN_POINT ( 'NONE',  ( -3.920142863837685177, 53.53904487068937357, 12.91830804447569214 ) ) ;
#9114 = VECTOR ( 'NONE', #14236, 1000.000000000000000 ) ;
#9115 = ADVANCED_FACE ( 'NONE', ( #1504 ), #2819, .F. ) ;
#9116 = CARTESIAN_POINT ( 'NONE',  ( -3.636496289402155746, 54.52999999999999403, 11.19198476289190936 ) ) ;
#9117 = CONTEXT_DEPENDENT_SHAPE_REPRESENTATION ( #10501, #14941 ) ;
#9118 = CARTESIAN_POINT ( 'NONE',  ( 4.171729424061791924, 78.03000000000000114, -12.83926296998457239 ) ) ;
#9119 = CARTESIAN_POINT ( 'NONE',  ( 13.22096164572512222, 51.52648539050532861, -2.730718222746924884 ) ) ;
#9120 = CARTESIAN_POINT ( 'NONE',  ( -13.46620905683853486, 37.89699380932566442, -0.9563560816646710094 ) ) ;
#9121 = CARTESIAN_POINT ( 'NONE',  ( 12.94672365821387139, 36.56709068650133787, -3.829332532818771284 ) ) ;
#9122 = CARTESIAN_POINT ( 'NONE',  ( -11.37499999999999645, -32.22499999999993747, -9.545674412382054647E-13 ) ) ;
#9123 = CARTESIAN_POINT ( 'NONE',  ( -6.083576914348308051, 74.45773797485220769, 12.05155980095794277 ) ) ;
#9124 = CARTESIAN_POINT ( 'NONE',  ( -9.236354345383572806, 77.31949598331318896, 9.855674949580887301 ) ) ;
#9125 = AXIS2_PLACEMENT_3D ( 'NONE', #9649, #14999, #16148 ) ;
#9126 = CARTESIAN_POINT ( 'NONE',  ( -6.741112569723631154, 80.43110928230144907, 11.69660190220037421 ) ) ;
#9127 = CARTESIAN_POINT ( 'NONE',  ( 7.500000000000000888, 106.7516370761002520, -7.534909587719530677 ) ) ;
#9128 = ORIENTED_EDGE ( 'NONE', *, *, #16431, .F. ) ;
#9129 = CARTESIAN_POINT ( 'NONE',  ( 7.272992578804311492, 8.880000000000000782, -10.01041549318726709 ) ) ;
#9130 = VERTEX_POINT ( 'NONE', #2466 ) ;
#9131 = CARTESIAN_POINT ( 'NONE',  ( -11.76794919243112325, 59.77999999999999403, -3.823638476888998827 ) ) ;
#9132 = CARTESIAN_POINT ( 'NONE',  ( 11.37500000000000178, -59.34999999999983800, 9.531744055041752924E-13 ) ) ;
#9133 = DIRECTION ( 'NONE',  ( 0.000000000000000000, 1.000000000000000000, 0.000000000000000000 ) ) ;
#9134 = CARTESIAN_POINT ( 'NONE',  ( 13.50000000000000000, -2.569999999999995843, 1.734723475976807094E-15 ) ) ;
#9135 = CARTESIAN_POINT ( 'NONE',  ( 8.559272513022497364, 75.85165812557318077, -10.43981238950174451 ) ) ;
#9136 = CYLINDRICAL_SURFACE ( 'NONE', #14152, 8.999999999999998224 ) ;
#9137 = CARTESIAN_POINT ( 'NONE',  ( 3.097840831347480339, 65.79138985724777910, 13.13976367567505754 ) ) ;
#9138 = CARTESIAN_POINT ( 'NONE',  ( -4.171729424061787483, 76.32999999999999829, -12.83926296998457417 ) ) ;
#9139 = CARTESIAN_POINT ( 'NONE',  ( -11.76794919243112325, 41.92999999999999261, -2.882316262207890869E-15 ) ) ;
#9140 = CARTESIAN_POINT ( 'NONE',  ( -9.708203932499419153, 9.763974596215597046, -7.053423027509717613 ) ) ;
#9141 = CIRCLE ( 'NONE', #1487, 4.000000000000004441 ) ;
#9142 = CARTESIAN_POINT ( 'NONE',  ( -9.988570099143858627, 59.28138111796381793, 9.081841899843952959 ) ) ;
#9143 = CARTESIAN_POINT ( 'NONE',  ( 9.161746794075217082, 45.03695357300266977, 9.915270584471830517 ) ) ;
#9144 = CARTESIAN_POINT ( 'NONE',  ( 13.50023044427028651, 69.41460068291787877, 0.4327633727389757490 ) ) ;
#9145 = DIRECTION ( 'NONE',  ( 0.000000000000000000, 1.000000000000000000, 0.000000000000000000 ) ) ;
#9146 = CARTESIAN_POINT ( 'NONE',  ( 13.08917948282296706, 30.54760429764663954, -3.305587359976819073 ) ) ;
#9147 = CARTESIAN_POINT ( 'NONE',  ( -11.19388950051994058, 55.64631903439251914, -7.546317585596763244 ) ) ;
#9148 = CARTESIAN_POINT ( 'NONE',  ( -13.49204055340601904, 49.94875050132303329, 0.5461732183256954309 ) ) ;
#9149 = CARTESIAN_POINT ( 'NONE',  ( 16.82677684650033356, 7.170662809914418290, -13.14483242576210742 ) ) ;
#9150 = CARTESIAN_POINT ( 'NONE',  ( 11.87714970433990658, 42.66748928331573154, -6.417526362764760961 ) ) ;
#9151 = CARTESIAN_POINT ( 'NONE',  ( 12.05894746113889937, 39.20340553057236832, 6.158319521186863099 ) ) ;
#9152 = ORIENTED_EDGE ( 'NONE', *, *, #2316, .T. ) ;
#9153 = CARTESIAN_POINT ( 'NONE',  ( -12.74992687881205811, 70.76992611378939557, -4.437291153396828669 ) ) ;
#9154 = CARTESIAN_POINT ( 'NONE',  ( -4.046715542471715388, 61.32550477582727666, -12.87921504933485650 ) ) ;
#9155 = CARTESIAN_POINT ( 'NONE',  ( 11.76794919243112325, 8.429999999999992610, 1.734723475976807094E-15 ) ) ;
#9156 = ORIENTED_EDGE ( 'NONE', *, *, #986, .T. ) ;
#9157 = ORIENTED_EDGE ( 'NONE', *, *, #10454, .F. ) ;
#9158 = CARTESIAN_POINT ( 'NONE',  ( -8.343458848123582072, 23.38000000000000966, 11.48378591275254124 ) ) ;
#9159 = CARTESIAN_POINT ( 'NONE',  ( -1.564113515457998572E-12, -79.08749999999980673, 18.62500000000000000 ) ) ;
#9160 = CARTESIAN_POINT ( 'NONE',  ( 2.044565740421548927, 61.10653920895618540, -13.35237565107692426 ) ) ;
#9161 = CARTESIAN_POINT ( 'NONE',  ( 13.49957401375394639, 57.43371563003871927, -0.1085156115176826724 ) ) ;
#9162 = CARTESIAN_POINT ( 'NONE',  ( -11.76794919243112325, 65.78000000000001535, -3.823638476888998827 ) ) ;
#9163 = CARTESIAN_POINT ( 'NONE',  ( 11.76794919243112680, 73.58000000000001251, -3.823638476888993942 ) ) ;
#9164 = EDGE_CURVE ( 'NONE', #9213, #2258, #10324, .T. ) ;
#9165 = CARTESIAN_POINT ( 'NONE',  ( -20.00000000000000000, 0.000000000000000000, -2.102236684100764122E-13 ) ) ;
#9166 = DIRECTION ( 'NONE',  ( 0.000000000000000000, 0.000000000000000000, -1.000000000000000000 ) ) ;
#9167 = DIRECTION ( 'NONE',  ( -9.637352644315595243E-17, 1.000000000000000000, 0.000000000000000000 ) ) ;
#9168 = CARTESIAN_POINT ( 'NONE',  ( -11.37500000000039613, -9.365624999999976552, 4.711679271993002516 ) ) ;
#9169 = DIRECTION ( 'NONE',  ( 1.000000000000000000, 0.000000000000000000, 0.000000000000000000 ) ) ;
#9170 = CARTESIAN_POINT ( 'NONE',  ( 3.123084801584079084, 34.06770800467356253, -13.13381235157419091 ) ) ;
#9171 = CARTESIAN_POINT ( 'NONE',  ( -3.648110378726476810, 73.31117878912979791, -12.99774238346768129 ) ) ;
#9172 = ORIENTED_EDGE ( 'NONE', *, *, #16392, .F. ) ;
#9173 = ORIENTED_EDGE ( 'NONE', *, *, #11084, .F. ) ;
#9174 = CARTESIAN_POINT ( 'NONE',  ( -11.76794919243112325, 74.92999999999999261, -2.882316262207890869E-15 ) ) ;
#9175 = ORIENTED_EDGE ( 'NONE', *, *, #11201, .T. ) ;
#9176 = CARTESIAN_POINT ( 'NONE',  ( 10.92172942406178926, 18.13000000000000611, 7.935100905948385908 ) ) ;
#9177 = CARTESIAN_POINT ( 'NONE',  ( -4.711679271993001628, -62.40312499999986073, -11.37500000000039613 ) ) ;
#9178 = CARTESIAN_POINT ( 'NONE',  ( -8.693204481589310362, 44.34575204853277341, 10.33905691976574559 ) ) ;
#9179 = CARTESIAN_POINT ( 'NONE',  ( -7.499999999999999112, -24.45288220904213361, -8.693347190813744518 ) ) ;
#9180 = CARTESIAN_POINT ( 'NONE',  ( 12.71166604806362166, 66.59423623445172780, -4.546593178848175043 ) ) ;
#9181 = CARTESIAN_POINT ( 'NONE',  ( 13.50000000000000000, 57.42999999999999261, 1.653273178848926867E-15 ) ) ;
#9182 = CARTESIAN_POINT ( 'NONE',  ( -3.964846123382400833, 71.53753483708018734, 12.90535649358312043 ) ) ;
#9183 = ADVANCED_FACE ( 'NONE', ( #9232 ), #1324, .F. ) ;
#9184 = CIRCLE ( 'NONE', #14503, 14.50000000000000000 ) ;
#9185 = CARTESIAN_POINT ( 'NONE',  ( 13.16986379959834075, -81.16874999999980389, 13.16986379960055231 ) ) ;
#9186 = CARTESIAN_POINT ( 'NONE',  ( -12.89466115481902975, 67.78656044428841199, -3.997873320072883097 ) ) ;
#9187 = CARTESIAN_POINT ( 'NONE',  ( -13.16986379960055231, -93.65624999999977263, 13.16986379959834252 ) ) ;
#9188 = CARTESIAN_POINT ( 'NONE',  ( 9.257325759640430363, 54.81840794441243503, -9.826123182423009084 ) ) ;
#9189 = CARTESIAN_POINT ( 'NONE',  ( 1.561832610794586538E-12, -70.76249999999983231, -18.62500000000000000 ) ) ;
#9190 = CARTESIAN_POINT ( 'NONE',  ( -5.186086855064643508, 65.49256697006511274, 12.46412873091786722 ) ) ;
#9191 = CARTESIAN_POINT ( 'NONE',  ( -3.070170608275790247, 62.56961157363158321, 13.15440911902680021 ) ) ;
#9192 = CARTESIAN_POINT ( 'NONE',  ( -6.686918715536896762, 35.43339511926818375, 11.73038437417416446 ) ) ;
#9193 = CARTESIAN_POINT ( 'NONE',  ( 8.343458848123578520, 18.98000000000000043, 11.48378591275254124 ) ) ;
#9194 = ORIENTED_EDGE ( 'NONE', *, *, #9973, .F. ) ;
#9195 = CYLINDRICAL_SURFACE ( 'NONE', #2766, 26.00000000000000355 ) ;
#9196 =( BOUNDED_SURFACE ( )  B_SPLINE_SURFACE ( 1, 2, ( 
 ( #4624, #12662, #7459, #13006, #15551, #6215, #551, #1865, #5961, #10199, #3543, #11341, #14062, #16718, #11686, #4966, #10370, #8877, #6049, #12841, #8616, #11602, #2116, #727, #13968, #10031, #15378, #10113, #6136, #2203, #16892, #4797, #7543, #10283, #12921, #15635, #8959, #14315, #15815, #10540, #6565, #8310, #10856, #4135, #9138, #7890, #14896, #3720, #1066, #9636, #5655, #1561, #11945, #17325, #6981, #14577, #2790, #14486, #5475, #14985, #978, #6478, #2286, #9046, #13582, #13092, #11037, #6892, #15902, #14398, #5150, #9224, #3811, #4222, #1475, #12265, #2373, #16224, #3632, #9547, #8221, #7808, #163, #5567, #13181, #17149, #11864, #10949, #12356, #17239, #16316, #2877, #2459, #7715, #13267, #13665, #1155, #250, #6390, #11773, #5061, #10456, #16673, #5915, #593, #681, #8658, #1988, #10073, #15424, #15067, #11294, #12447, #2967, #5828, #3331, #4579, #15158, #3057, #12706, #6004, #8570, #15247, #8396, #11211, #9986, #7413, #16585, #6093, #11386, #332, #8485, #9722, #14103, #12795, #16409, #15334, #11122, #3145, #8746, #14013, #3237, #13923, #4310, #13750, #5741, #13836, #1817, #1649, #7065, #16497, #1905, #7322, #4402, #7232, #16759, #12619, #9812, #4490, #507, #1736, #4666, #7149, #12534, #420, #9900, #11560, #8917, #17199, #13223, #9181, #2245, #7673, #14530, #4926, #10413, #16935, #13052, #5107, #8834, #14275, #10158, #16850, #3679, #3420, #1111, #14447, #846, #4752, #12964, #17022, #11644, #11820, #9095, #2333, #4838, #935, #11474, #6344, #14357, #15595, #15770, #13138, #3502, #7500, #2161, #7767, #2416, #10241, #11730, #17107, #6257, #15508, #7585, #10499, #15680, #1026, #6436, #15862, #10325, #3769, #5013, #7849, #14191, #2075, #12881, #769, #6177, #3587, #8999, #13476, #2505, #5196, #13390, #10930, #12158, #5285, #10668, #2767, #8199, #16115, #5366, #10584, #1279, #49, #14967, #6692, #13647, #1453, #7935, #16032, #1363, #4114, #15945, #17282, #3854, #8112, #2592, #10837, #9529, #14872, #17370, #12246, #6780, #5453, #13563, #8290, #16203, #9616, #140, #5546, #9268, #6871, #13308, #14620, #12073, #16297, #4205, #3940, #9354, #2858, #6526, #4026, #10751, #1198, #17452, #11905, #6610, #9441, #11989, #14703, #8022, #14789, #2679, #16653, #230, #12338, #5636, #3127, #12518, #5984, #402, #8639, #16740, #4646, #10052, #13905, #13734, #5810, #576, #11276, #8553, #11193, #15402, #11018, #15051, #11104, #16569, #12686, #16389, #4293, #12601, #4560, #9705, #4475, #1801, #9881, #1631, #8467, #15230, #11366, #7213, #490, #7049, #5896, #9966, #12428, #16478, #7301, #3310, #8723, #15315, #3217, #1541, #13990, #1887, #314, #6959, #2949, #8377, #4383, #5723, #9791, #15138, #3036 ),
 ( #13818, #1719, #7131, #8983, #17000, #751, #916, #15750, #6159, #10135, #11536, #4994, #5089, #14170, #15659, #14338, #15573, #661, #10220, #2314, #827, #13032, #16914, #13117, #4819, #12862, #6416, #3747, #3484, #6325, #15489, #7481, #3399, #4906, #2058, #16827, #2227, #7656, #6071, #8899, #11801, #17177, #14253, #7393, #11453, #10395, #10481, #15841, #2141, #7566, #12943, #11711, #14082, #4734, #12773, #8812, #6238, #1005, #14425, #3568, #7742, #11625, #1969, #10305, #17088, #3661, #9072, #5174, #10908, #6848, #17262, #1180, #5524, #6591, #5429, #11971, #4093, #2573, #1342, #16013, #2397, #16181, #9336, #9422, #11888, #13455, #17352, #7917, #5264, #6506, #26, #12226, #14853, #10566, #15926, #13371, #10819, #8091, #14686, #10650, #8005, #1431, #1260, #7832, #13205, #2747, #3836, #12137, #12055, #1091, #6758, #13291, #9250, #14603, #118, #9508, #2483, #2661, #16277, #8178, #13541, #9162, #5346, #3919, #14510, #6672, #17433, #10733, #16097, #4005, #14770, #552, #7028, #13882, #7193, #8443, #7280, #11172, #11342, #4539, #7111, #3107, #1611, #5877, #9769, #3196, #210, #15032, #4453, #13712, #1866, #12663, #5962, #16547, #16365, #3013, #8617, #1783, #9860, #13798, #4183, #2837, #5615, #12406, #1696, #15294, #13629, #1521, #15207, #12581, #12316, #12495, #8534, #382, #4273, #11085, #5787, #13971, #469, #11256, #9682, #16635, #9946, #2925, #294, #9595, #14947, #8268, #6938, #10997, #8355, #15115, #5703, #16458, #4360, #4968, #14063, #14147, #15380, #4625, #8960, #8702, #6392, #2204, #6137, #10032, #729, #4798, #16894, #17064, #14316, #7630, #10115, #12922, #16719, #11603, #2118, #3377, #3545, #889, #8789, #12750, #2035, #13008, #7716, #16804, #806, #16979, #11516, #3288, #12842, #10371, #3463, #15636, #6301, #11687, #15467, #15725, #4881, #6217, #3633, #979, #9047, #2288, #14399, #13093, #1947, #10284, #637, #7371, #10200, #6050, #11433, #7460, #15552, #4711, #8878, #14232, #7544, #10457, #6566, #17410, #2724, #11946, #1408, #6735, #7809, #3812, #1237, #9397, #15817, #5062, #3721, #13348, #5238, #16159, #10624, #1319, #14830, #1156, #9139, #14487, #2636, #9484, #8152, #10541, #17326, #15903, #14747, #4069, #2374, #13182, #1067, #9225, #10795, #12114, #6649, #5408, #15989, #17150, #11774, #3893, #10709, #7891, #6479, #13517, #11865, #17240, #14579, #5151, #2460, #8067, #13268, #3, #9311, #3982, #14661, #2549, #7979, #12031, #5325, #16075, #13431, #4248, #5592, #2899, #4157, #15182, #4514, #12558, #14920, #8244, #11059, #3083, #5762, #7003, #16340, #12379, #16610, #5679, #94, #5499, #443, #13604, #9836, #9744, #10882, #16521, #10972, #16252, #1499, #9922, #11145, #9570, #356 ) ),
 .UNSPECIFIED., .F., .F., .F. ) 
 B_SPLINE_SURFACE_WITH_KNOTS ( ( 2, 2 ),
 ( 3, 2, 2, 2, 2, 2, 2, 2, 2, 2, 2, 2, 2, 2, 2, 2, 2, 2, 2, 2, 2, 2, 2, 2, 2, 2, 2, 2, 2, 2, 2, 2, 2, 2, 2, 2, 2, 2, 2, 2, 2, 2, 2, 2, 2, 2, 2, 2, 2, 2, 2, 2, 2, 2, 2, 2, 2, 2, 2, 2, 2, 2, 2, 2, 2, 2, 2, 2, 2, 2, 2, 2, 2, 2, 2, 2, 2, 2, 2, 2, 2, 2, 2, 2, 2, 2, 2, 2, 2, 2, 2, 2, 2, 2, 2, 2, 2, 2, 2, 2, 2, 2, 2, 2, 2, 2, 2, 2, 2, 2, 2, 2, 2, 2, 2, 2, 2, 2, 2, 2, 2, 2, 2, 2, 2, 2, 2, 2, 2, 2, 2, 2, 2, 2, 2, 2, 2, 2, 2, 2, 2, 2, 2, 2, 2, 2, 2, 2, 2, 2, 2, 2, 2, 2, 2, 2, 2, 2, 2, 2, 2, 2, 2, 2, 2, 2, 2, 2, 2, 2, 2, 2, 2, 2, 2, 2, 2, 3 ),
 ( 0.000000000000000000, 1.000000000000000000 ),
 ( 0.000000000000000000, 0.005555555555555555768, 0.01111111111111111154, 0.01666666666666666644, 0.02222222222222222307, 0.02777777777777777624, 0.03333333333333333287, 0.03888888888888888951, 0.04444444444444444614, 0.05000000000000000278, 0.05555555555555555247, 0.06111111111111110911, 0.06666666666666666574, 0.07222222222222221544, 0.07777777777777777901, 0.08333333333333332871, 0.08888888888888889228, 0.09444444444444444198, 0.1000000000000000056, 0.1055555555555555552, 0.1111111111111111049, 0.1166666666666666685, 0.1222222222222222182, 0.1277777777777777679, 0.1333333333333333315, 0.1388888888888888951, 0.1444444444444444309, 0.1499999999999999944, 0.1555555555555555580, 0.1611111111111111216, 0.1666666666666666574, 0.1722222222222222210, 0.1777777777777777846, 0.1833333333333333204, 0.1888888888888888840, 0.1944444444444444475, 0.2000000000000000111, 0.2055555555555555469, 0.2111111111111111105, 0.2166666666666666741, 0.2222222222222222099, 0.2277777777777777735, 0.2333333333333333370, 0.2388888888888889006, 0.2444444444444444364, 0.2500000000000000000, 0.2555555555555555358, 0.2611111111111111271, 0.2666666666666666630, 0.2722222222222221988, 0.2777777777777777901, 0.2833333333333333259, 0.2888888888888888618, 0.2944444444444444531, 0.2999999999999999889, 0.3055555555555555802, 0.3111111111111111160, 0.3166666666666666519, 0.3222222222222222432, 0.3277777777777777790, 0.3333333333333333148, 0.3388888888888889062, 0.3444444444444444420, 0.3499999999999999778, 0.3555555555555555691, 0.3611111111111111049, 0.3666666666666666408, 0.3722222222222222321, 0.3777777777777777679, 0.3833333333333333592, 0.3888888888888888951, 0.3944444444444444309, 0.4000000000000000222, 0.4055555555555555580, 0.4111111111111110938, 0.4166666666666666852, 0.4222222222222222210, 0.4277777777777777568, 0.4333333333333333481, 0.4388888888888888840, 0.4444444444444444198, 0.4500000000000000111, 0.4555555555555555469, 0.4611111111111111382, 0.4666666666666666741, 0.4722222222222222099, 0.4777777777777778012, 0.4833333333333333370, 0.4888888888888888729, 0.4944444444444444642, 0.5000000000000000000, 0.5055555555555555358, 0.5111111111111110716, 0.5166666666666667185, 0.5222222222222222543, 0.5277777777777777901, 0.5333333333333333259, 0.5388888888888888618, 0.5444444444444443976, 0.5500000000000000444, 0.5555555555555555802, 0.5611111111111111160, 0.5666666666666666519, 0.5722222222222221877, 0.5777777777777777235, 0.5833333333333333703, 0.5888888888888889062, 0.5944444444444444420, 0.5999999999999999778, 0.6055555555555555136, 0.6111111111111111605, 0.6166666666666666963, 0.6222222222222222321, 0.6277777777777777679, 0.6333333333333333037, 0.6388888888888888395, 0.6444444444444444864, 0.6500000000000000222, 0.6555555555555555580, 0.6611111111111110938, 0.6666666666666666297, 0.6722222222222222765, 0.6777777777777778123, 0.6833333333333333481, 0.6888888888888888840, 0.6944444444444444198, 0.6999999999999999556, 0.7055555555555556024, 0.7111111111111111382, 0.7166666666666666741, 0.7222222222222222099, 0.7277777777777777457, 0.7333333333333332815, 0.7388888888888889284, 0.7444444444444444642, 0.7500000000000000000, 0.7555555555555555358, 0.7611111111111110716, 0.7666666666666667185, 0.7722222222222222543, 0.7777777777777777901, 0.7833333333333333259, 0.7888888888888888618, 0.7944444444444443976, 0.8000000000000000444, 0.8055555555555555802, 0.8111111111111111160, 0.8166666666666666519, 0.8222222222222221877, 0.8277777777777777235, 0.8333333333333333703, 0.8388888888888889062, 0.8444444444444444420, 0.8499999999999999778, 0.8555555555555555136, 0.8611111111111111605, 0.8666666666666666963, 0.8722222222222222321, 0.8777777777777777679, 0.8833333333333333037, 0.8888888888888888395, 0.8944444444444444864, 0.9000000000000000222, 0.9055555555555555580, 0.9111111111111110938, 0.9166666666666666297, 0.9222222222222222765, 0.9277777777777778123, 0.9333333333333333481, 0.9388888888888888840, 0.9444444444444444198, 0.9499999999999999556, 0.9555555555555556024, 0.9611111111111111382, 0.9666666666666666741, 0.9722222222222222099, 0.9777777777777777457, 0.9814746806989694816 ),
 .UNSPECIFIED. ) 
 GEOMETRIC_REPRESENTATION_ITEM ( )  RATIONAL_B_SPLINE_SURFACE ( (
 ( 1.000000000000000000, 0.9510565162951535312, 1.000000000000000000, 0.9510565162951535312, 1.000000000000000000, 0.9510565162951535312, 1.000000000000000000, 0.9510565162951535312, 1.000000000000000000, 0.9510565162951535312, 1.000000000000000000, 0.9510565162951535312, 1.000000000000000000, 0.9510565162951535312, 1.000000000000000000, 0.9510565162951535312, 1.000000000000000000, 0.9510565162951535312, 1.000000000000000000, 0.9510565162951535312, 1.000000000000000000, 0.9510565162951535312, 1.000000000000000000, 0.9510565162951535312, 1.000000000000000000, 0.9510565162951535312, 1.000000000000000000, 0.9510565162951535312, 1.000000000000000000, 0.9510565162951535312, 1.000000000000000000, 0.9510565162951535312, 1.000000000000000000, 0.9510565162951535312, 1.000000000000000000, 0.9510565162951535312, 1.000000000000000000, 0.9510565162951535312, 1.000000000000000000, 0.9510565162951535312, 1.000000000000000000, 0.9510565162951535312, 1.000000000000000000, 0.9510565162951535312, 1.000000000000000000, 0.9510565162951535312, 1.000000000000000000, 0.9510565162951535312, 1.000000000000000000, 0.9510565162951535312, 1.000000000000000000, 0.9510565162951535312, 1.000000000000000000, 0.9510565162951535312, 1.000000000000000000, 0.9510565162951535312, 1.000000000000000000, 0.9510565162951535312, 1.000000000000000000, 0.9510565162951535312, 1.000000000000000000, 0.9510565162951535312, 1.000000000000000000, 0.9510565162951535312, 1.000000000000000000, 0.9510565162951535312, 1.000000000000000000, 0.9510565162951535312, 1.000000000000000000, 0.9510565162951535312, 1.000000000000000000, 0.9510565162951535312, 1.000000000000000000, 0.9510565162951535312, 1.000000000000000000, 0.9510565162951535312, 1.000000000000000000, 0.9510565162951535312, 1.000000000000000000, 0.9510565162951535312, 1.000000000000000000, 0.9510565162951535312, 1.000000000000000000, 0.9510565162951535312, 1.000000000000000000, 0.9510565162951535312, 1.000000000000000000, 0.9510565162951535312, 1.000000000000000000, 0.9510565162951535312, 1.000000000000000000, 0.9510565162951535312, 1.000000000000000000, 0.9510565162951535312, 1.000000000000000000, 0.9510565162951535312, 1.000000000000000000, 0.9510565162951535312, 1.000000000000000000, 0.9510565162951535312, 1.000000000000000000, 0.9510565162951535312, 1.000000000000000000, 0.9510565162951535312, 1.000000000000000000, 0.9510565162951535312, 1.000000000000000000, 0.9510565162951535312, 1.000000000000000000, 0.9510565162951535312, 1.000000000000000000, 0.9510565162951535312, 1.000000000000000000, 0.9510565162951535312, 1.000000000000000000, 0.9510565162951535312, 1.000000000000000000, 0.9510565162951535312, 1.000000000000000000, 0.9510565162951535312, 1.000000000000000000, 0.9510565162951535312, 1.000000000000000000, 0.9510565162951535312, 1.000000000000000000, 0.9510565162951535312, 1.000000000000000000, 0.9510565162951535312, 1.000000000000000000, 0.9510565162951535312, 1.000000000000000000, 0.9510565162951535312, 1.000000000000000000, 0.9510565162951535312, 1.000000000000000000, 0.9510565162951535312, 1.000000000000000000, 0.9510565162951535312, 1.000000000000000000, 0.9510565162951535312, 1.000000000000000000, 0.9510565162951535312, 1.000000000000000000, 0.9510565162951535312, 1.000000000000000000, 0.9510565162951535312, 1.000000000000000000, 0.9510565162951535312, 1.000000000000000000, 0.9510565162951535312, 1.000000000000000000, 0.9510565162951535312, 1.000000000000000000, 0.9510565162951535312, 1.000000000000000000, 0.9510565162951535312, 1.000000000000000000, 0.9510565162951535312, 1.000000000000000000, 0.9510565162951535312, 1.000000000000000000, 0.9510565162951535312, 1.000000000000000000, 0.9510565162951535312, 1.000000000000000000, 0.9510565162951535312, 1.000000000000000000, 0.9510565162951535312, 1.000000000000000000, 0.9510565162951535312, 1.000000000000000000, 0.9510565162951535312, 1.000000000000000000, 0.9510565162951535312, 1.000000000000000000, 0.9510565162951535312, 1.000000000000000000, 0.9510565162951535312, 1.000000000000000000, 0.9510565162951535312, 1.000000000000000000, 0.9510565162951535312, 1.000000000000000000, 0.9510565162951535312, 1.000000000000000000, 0.9510565162951535312, 1.000000000000000000, 0.9510565162951535312, 1.000000000000000000, 0.9510565162951535312, 1.000000000000000000, 0.9510565162951535312, 1.000000000000000000, 0.9510565162951535312, 1.000000000000000000, 0.9510565162951535312, 1.000000000000000000, 0.9510565162951535312, 1.000000000000000000, 0.9510565162951535312, 1.000000000000000000, 0.9510565162951535312, 1.000000000000000000, 0.9510565162951535312, 1.000000000000000000, 0.9510565162951535312, 1.000000000000000000, 0.9510565162951535312, 1.000000000000000000, 0.9510565162951535312, 1.000000000000000000, 0.9510565162951535312, 1.000000000000000000, 0.9510565162951535312, 1.000000000000000000, 0.9510565162951535312, 1.000000000000000000, 0.9510565162951535312, 1.000000000000000000, 0.9510565162951535312, 1.000000000000000000, 0.9510565162951535312, 1.000000000000000000, 0.9510565162951535312, 1.000000000000000000, 0.9510565162951535312, 1.000000000000000000, 0.9510565162951535312, 1.000000000000000000, 0.9510565162951535312, 1.000000000000000000, 0.9510565162951535312, 1.000000000000000000, 0.9510565162951535312, 1.000000000000000000, 0.9510565162951535312, 1.000000000000000000, 0.9510565162951535312, 1.000000000000000000, 0.9510565162951535312, 1.000000000000000000, 0.9510565162951535312, 1.000000000000000000, 0.9510565162951535312, 1.000000000000000000, 0.9510565162951535312, 1.000000000000000000, 0.9510565162951535312, 1.000000000000000000, 0.9510565162951535312, 1.000000000000000000, 0.9510565162951535312, 1.000000000000000000, 0.9510565162951535312, 1.000000000000000000, 0.9510565162951535312, 1.000000000000000000, 0.9510565162951535312, 1.000000000000000000, 0.9510565162951535312, 1.000000000000000000, 0.9510565162951535312, 1.000000000000000000, 0.9510565162951535312, 1.000000000000000000, 0.9510565162951535312, 1.000000000000000000, 0.9510565162951535312, 1.000000000000000000, 0.9510565162951535312, 1.000000000000000000, 0.9510565162951535312, 1.000000000000000000, 0.9510565162951535312, 1.000000000000000000, 0.9510565162951535312, 1.000000000000000000, 0.9510565162951535312, 1.000000000000000000, 0.9510565162951535312, 1.000000000000000000, 0.9510565162951535312, 1.000000000000000000, 0.9510565162951535312, 1.000000000000000000, 0.9510565162951535312, 1.000000000000000000, 0.9510565162951535312, 1.000000000000000000, 0.9510565162951535312, 1.000000000000000000, 0.9510565162951535312, 1.000000000000000000, 0.9510565162951535312, 1.000000000000000000, 0.9510565162951535312, 1.000000000000000000, 0.9510565162951535312, 1.000000000000000000, 0.9510565162951535312, 1.000000000000000000, 0.9510565162951535312, 1.000000000000000000, 0.9510565162951535312, 1.000000000000000000, 0.9510565162951535312, 1.000000000000000000, 0.9510565162951535312, 1.000000000000000000, 0.9510565162951535312, 1.000000000000000000, 0.9510565162951535312, 1.000000000000000000, 0.9510565162951535312, 1.000000000000000000, 0.9510565162951535312, 1.000000000000000000, 0.9510565162951535312, 1.000000000000000000, 0.9510565162951535312, 1.000000000000000000, 0.9510565162951535312, 1.000000000000000000, 0.9510565162951535312, 1.000000000000000000, 0.9510565162951535312, 1.000000000000000000, 0.9510565162951535312, 1.000000000000000000, 0.9510565162951535312, 1.000000000000000000, 0.9510565162951535312, 1.000000000000000000, 0.9510565162951535312, 1.000000000000000000, 0.9510565162951535312, 1.000000000000000000, 0.9510565162951535312, 1.000000000000000000, 0.9510565162951535312, 1.000000000000000000, 0.9510565162951535312, 1.000000000000000000, 0.9510565162951535312, 1.000000000000000000, 0.9510565162951535312, 1.000000000000000000, 0.9510565162951535312, 1.000000000000000000, 0.9510565162951535312, 1.000000000000000000, 0.9510565162951535312, 1.000000000000000000, 0.9674309245812854341, 0.9782075447827165426),
 ( 1.000000000000000000, 0.9510565162951535312, 1.000000000000000000, 0.9510565162951535312, 1.000000000000000000, 0.9510565162951535312, 1.000000000000000000, 0.9510565162951535312, 1.000000000000000000, 0.9510565162951535312, 1.000000000000000000, 0.9510565162951535312, 1.000000000000000000, 0.9510565162951535312, 1.000000000000000000, 0.9510565162951535312, 1.000000000000000000, 0.9510565162951535312, 1.000000000000000000, 0.9510565162951535312, 1.000000000000000000, 0.9510565162951535312, 1.000000000000000000, 0.9510565162951535312, 1.000000000000000000, 0.9510565162951535312, 1.000000000000000000, 0.9510565162951535312, 1.000000000000000000, 0.9510565162951535312, 1.000000000000000000, 0.9510565162951535312, 1.000000000000000000, 0.9510565162951535312, 1.000000000000000000, 0.9510565162951535312, 1.000000000000000000, 0.9510565162951535312, 1.000000000000000000, 0.9510565162951535312, 1.000000000000000000, 0.9510565162951535312, 1.000000000000000000, 0.9510565162951535312, 1.000000000000000000, 0.9510565162951535312, 1.000000000000000000, 0.9510565162951535312, 1.000000000000000000, 0.9510565162951535312, 1.000000000000000000, 0.9510565162951535312, 1.000000000000000000, 0.9510565162951535312, 1.000000000000000000, 0.9510565162951535312, 1.000000000000000000, 0.9510565162951535312, 1.000000000000000000, 0.9510565162951535312, 1.000000000000000000, 0.9510565162951535312, 1.000000000000000000, 0.9510565162951535312, 1.000000000000000000, 0.9510565162951535312, 1.000000000000000000, 0.9510565162951535312, 1.000000000000000000, 0.9510565162951535312, 1.000000000000000000, 0.9510565162951535312, 1.000000000000000000, 0.9510565162951535312, 1.000000000000000000, 0.9510565162951535312, 1.000000000000000000, 0.9510565162951535312, 1.000000000000000000, 0.9510565162951535312, 1.000000000000000000, 0.9510565162951535312, 1.000000000000000000, 0.9510565162951535312, 1.000000000000000000, 0.9510565162951535312, 1.000000000000000000, 0.9510565162951535312, 1.000000000000000000, 0.9510565162951535312, 1.000000000000000000, 0.9510565162951535312, 1.000000000000000000, 0.9510565162951535312, 1.000000000000000000, 0.9510565162951535312, 1.000000000000000000, 0.9510565162951535312, 1.000000000000000000, 0.9510565162951535312, 1.000000000000000000, 0.9510565162951535312, 1.000000000000000000, 0.9510565162951535312, 1.000000000000000000, 0.9510565162951535312, 1.000000000000000000, 0.9510565162951535312, 1.000000000000000000, 0.9510565162951535312, 1.000000000000000000, 0.9510565162951535312, 1.000000000000000000, 0.9510565162951535312, 1.000000000000000000, 0.9510565162951535312, 1.000000000000000000, 0.9510565162951535312, 1.000000000000000000, 0.9510565162951535312, 1.000000000000000000, 0.9510565162951535312, 1.000000000000000000, 0.9510565162951535312, 1.000000000000000000, 0.9510565162951535312, 1.000000000000000000, 0.9510565162951535312, 1.000000000000000000, 0.9510565162951535312, 1.000000000000000000, 0.9510565162951535312, 1.000000000000000000, 0.9510565162951535312, 1.000000000000000000, 0.9510565162951535312, 1.000000000000000000, 0.9510565162951535312, 1.000000000000000000, 0.9510565162951535312, 1.000000000000000000, 0.9510565162951535312, 1.000000000000000000, 0.9510565162951535312, 1.000000000000000000, 0.9510565162951535312, 1.000000000000000000, 0.9510565162951535312, 1.000000000000000000, 0.9510565162951535312, 1.000000000000000000, 0.9510565162951535312, 1.000000000000000000, 0.9510565162951535312, 1.000000000000000000, 0.9510565162951535312, 1.000000000000000000, 0.9510565162951535312, 1.000000000000000000, 0.9510565162951535312, 1.000000000000000000, 0.9510565162951535312, 1.000000000000000000, 0.9510565162951535312, 1.000000000000000000, 0.9510565162951535312, 1.000000000000000000, 0.9510565162951535312, 1.000000000000000000, 0.9510565162951535312, 1.000000000000000000, 0.9510565162951535312, 1.000000000000000000, 0.9510565162951535312, 1.000000000000000000, 0.9510565162951535312, 1.000000000000000000, 0.9510565162951535312, 1.000000000000000000, 0.9510565162951535312, 1.000000000000000000, 0.9510565162951535312, 1.000000000000000000, 0.9510565162951535312, 1.000000000000000000, 0.9510565162951535312, 1.000000000000000000, 0.9510565162951535312, 1.000000000000000000, 0.9510565162951535312, 1.000000000000000000, 0.9510565162951535312, 1.000000000000000000, 0.9510565162951535312, 1.000000000000000000, 0.9510565162951535312, 1.000000000000000000, 0.9510565162951535312, 1.000000000000000000, 0.9510565162951535312, 1.000000000000000000, 0.9510565162951535312, 1.000000000000000000, 0.9510565162951535312, 1.000000000000000000, 0.9510565162951535312, 1.000000000000000000, 0.9510565162951535312, 1.000000000000000000, 0.9510565162951535312, 1.000000000000000000, 0.9510565162951535312, 1.000000000000000000, 0.9510565162951535312, 1.000000000000000000, 0.9510565162951535312, 1.000000000000000000, 0.9510565162951535312, 1.000000000000000000, 0.9510565162951535312, 1.000000000000000000, 0.9510565162951535312, 1.000000000000000000, 0.9510565162951535312, 1.000000000000000000, 0.9510565162951535312, 1.000000000000000000, 0.9510565162951535312, 1.000000000000000000, 0.9510565162951535312, 1.000000000000000000, 0.9510565162951535312, 1.000000000000000000, 0.9510565162951535312, 1.000000000000000000, 0.9510565162951535312, 1.000000000000000000, 0.9510565162951535312, 1.000000000000000000, 0.9510565162951535312, 1.000000000000000000, 0.9510565162951535312, 1.000000000000000000, 0.9510565162951535312, 1.000000000000000000, 0.9510565162951535312, 1.000000000000000000, 0.9510565162951535312, 1.000000000000000000, 0.9510565162951535312, 1.000000000000000000, 0.9510565162951535312, 1.000000000000000000, 0.9510565162951535312, 1.000000000000000000, 0.9510565162951535312, 1.000000000000000000, 0.9510565162951535312, 1.000000000000000000, 0.9510565162951535312, 1.000000000000000000, 0.9510565162951535312, 1.000000000000000000, 0.9510565162951535312, 1.000000000000000000, 0.9510565162951535312, 1.000000000000000000, 0.9510565162951535312, 1.000000000000000000, 0.9510565162951535312, 1.000000000000000000, 0.9510565162951535312, 1.000000000000000000, 0.9510565162951535312, 1.000000000000000000, 0.9510565162951535312, 1.000000000000000000, 0.9510565162951535312, 1.000000000000000000, 0.9510565162951535312, 1.000000000000000000, 0.9510565162951535312, 1.000000000000000000, 0.9510565162951535312, 1.000000000000000000, 0.9510565162951535312, 1.000000000000000000, 0.9510565162951535312, 1.000000000000000000, 0.9510565162951535312, 1.000000000000000000, 0.9510565162951535312, 1.000000000000000000, 0.9510565162951535312, 1.000000000000000000, 0.9510565162951535312, 1.000000000000000000, 0.9510565162951535312, 1.000000000000000000, 0.9510565162951535312, 1.000000000000000000, 0.9510565162951535312, 1.000000000000000000, 0.9510565162951535312, 1.000000000000000000, 0.9510565162951535312, 1.000000000000000000, 0.9510565162951535312, 1.000000000000000000, 0.9510565162951535312, 1.000000000000000000, 0.9510565162951535312, 1.000000000000000000, 0.9510565162951535312, 1.000000000000000000, 0.9510565162951535312, 1.000000000000000000, 0.9510565162951535312, 1.000000000000000000, 0.9510565162951535312, 1.000000000000000000, 0.9510565162951535312, 1.000000000000000000, 0.9510565162951535312, 1.000000000000000000, 0.9510565162951535312, 1.000000000000000000, 0.9510565162951535312, 1.000000000000000000, 0.9510565162951535312, 1.000000000000000000, 0.9510565162951535312, 1.000000000000000000, 0.9510565162951535312, 1.000000000000000000, 0.9510565162951535312, 1.000000000000000000, 0.9510565162951535312, 1.000000000000000000, 0.9510565162951535312, 1.000000000000000000, 0.9510565162951535312, 1.000000000000000000, 0.9510565162951535312, 1.000000000000000000, 0.9510565162951535312, 1.000000000000000000, 0.9510565162951535312, 1.000000000000000000, 0.9510565162951535312, 1.000000000000000000, 0.9510565162951535312, 1.000000000000000000, 0.9674309245812854341, 0.9782075447827165426) ) ) 
 REPRESENTATION_ITEM ( '' )  SURFACE ( )  );
#9197 = CARTESIAN_POINT ( 'NONE',  ( -11.72349227228382773, 32.17874275710667575, 6.697393093110406426 ) ) ;
#9198 = CARTESIAN_POINT ( 'NONE',  ( 0.5398279591931279819, 73.16058978026926241, -13.48920530192332556 ) ) ;
#9199 = CARTESIAN_POINT ( 'NONE',  ( 13.49981200716974428, 60.43253933153254565, -0.07419703893695323016 ) ) ;
#9200 = CARTESIAN_POINT ( 'NONE',  ( 2.621994543952811015E-15, -6.820000000000003837, -14.19474002721660355 ) ) ;
#9201 = CARTESIAN_POINT ( 'NONE',  ( -7.043910900581732193, 53.41849667041662286, 11.51668441602786608 ) ) ;
#9202 = CARTESIAN_POINT ( 'NONE',  ( -11.76794919243112325, 53.77999999999999403, -3.823638476888998827 ) ) ;
#9203 = CARTESIAN_POINT ( 'NONE',  ( -4.171729424061787483, 72.33000000000001251, -12.83926296998457417 ) ) ;
#9204 = CARTESIAN_POINT ( 'NONE',  ( 12.78586417785842322, 51.27373664802115627, 4.335848610435731665 ) ) ;
#9205 = CARTESIAN_POINT ( 'NONE',  ( -13.38432117154441414, 37.99212082524375944, 1.778969478457535169 ) ) ;
#9206 = CARTESIAN_POINT ( 'NONE',  ( 9.963063945987066461, 36.78277068231086844, -9.111627411219474837 ) ) ;
#9207 = CARTESIAN_POINT ( 'NONE',  ( -4.711679271994915652, -35.34687499999993321, 11.37499999999960210 ) ) ;
#9208 = CARTESIAN_POINT ( 'NONE',  ( -0.8228155029539212517, 74.65041598456849670, 13.47518950460405840 ) ) ;
#9209 = AXIS2_PLACEMENT_3D ( 'NONE', #9108, #15609, #3349 ) ;
#9210 = CARTESIAN_POINT ( 'NONE',  ( -3.778147517876603079, 77.54415174377176356, 12.96054201803634776 ) ) ;
#9211 = CARTESIAN_POINT ( 'NONE',  ( -13.39192495110588865, 79.99130628515160879, 1.760924835796330301 ) ) ;
#9212 = CARTESIAN_POINT ( 'NONE',  ( 7.499999999999998224, 108.6229112031126220, 2.544524385544284950 ) ) ;
#9213 = VERTEX_POINT ( 'NONE', #2641 ) ;
#9214 = CARTESIAN_POINT ( 'NONE',  ( 0.000000000000000000, 5.918584287042170544, 0.000000000000000000 ) ) ;
#9215 = CARTESIAN_POINT ( 'NONE',  ( 3.636496289402154414, 7.830000000000003624, 11.19198476289190758 ) ) ;
#9216 = ADVANCED_FACE ( 'NONE', ( #8072 ), #13437, .T. ) ;
#9217 = VERTEX_POINT ( 'NONE', #16942 ) ;
#9218 = CARTESIAN_POINT ( 'NONE',  ( -7.272992578804310604, 60.37999999999998835, 10.01041549318726886 ) ) ;
#9219 = CARTESIAN_POINT ( 'NONE',  ( 8.043339635996302306, -73.91874999999977547, 8.043339635997654113 ) ) ;
#9220 = DIRECTION ( 'NONE',  ( 0.000000000000000000, 0.000000000000000000, -1.000000000000000000 ) ) ;
#9221 = CARTESIAN_POINT ( 'NONE',  ( 2.621994543952811015E-15, -7.820000000000002061, -14.19474002721660355 ) ) ;
#9222 = CARTESIAN_POINT ( 'NONE',  ( 7.500632703326952644, 75.89905631385393292, -11.22916880707215803 ) ) ;
#9223 = CARTESIAN_POINT ( 'NONE',  ( 2.138189944381220897, 69.10311857767972299, -13.50000000000000355 ) ) ;
#9224 = CARTESIAN_POINT ( 'NONE',  ( 13.49999999999999822, 72.28000000000000114, 4.386415899144237684 ) ) ;
#9225 = CARTESIAN_POINT ( 'NONE',  ( 7.272992578804308828, 39.97999999999999687, 10.01041549318726709 ) ) ;
#9226 = CARTESIAN_POINT ( 'NONE',  ( 19.29752010712851984, 5.918584287042171432, -17.42428528562851042 ) ) ;
#9227 = CARTESIAN_POINT ( 'NONE',  ( -3.112950329740383548, 58.29192748187959694, -13.14439478270550943 ) ) ;
#9228 = CARTESIAN_POINT ( 'NONE',  ( 11.46681240161533744, 45.16376727946777692, 7.124761802481938133 ) ) ;
#9229 = CARTESIAN_POINT ( 'NONE',  ( 13.47894498165622146, 69.39940522213998975, 0.8726673866746849084 ) ) ;
#9230 = B_SPLINE_CURVE_WITH_KNOTS ( 'NONE', 3,
 ( #16320, #1480, #13927, #8402, #12270, #13669, #167, #7237, #5571, #511, #10954, #5919, #12360, #254, #13754, #2971, #1653, #16677 ),
 .UNSPECIFIED., .F., .F.,
 ( 4, 2, 2, 2, 2, 2, 2, 2, 4 ),
 ( 2.030049010680398225E-07, 0.0005272941439305965910, 0.001054385282960125297, 0.001581476421989653786, 0.002108567561019182492, 0.002635658700048711198, 0.003162749839078239471, 0.003689840978107768177, 0.004216932117137296883 ),
 .UNSPECIFIED. ) ;
#9231 = CARTESIAN_POINT ( 'NONE',  ( -7.416407864998736166, 6.613974596215566493, -10.20780970022448031 ) ) ;
#9232 = FACE_OUTER_BOUND ( 'NONE', #6293, .T. ) ;
#9233 = CARTESIAN_POINT ( 'NONE',  ( -0.9607546724729691956, 55.21454159585901778, -13.46853932749331761 ) ) ;
#9234 = CARTESIAN_POINT ( 'NONE',  ( -5.721006742059940642, 50.47200087032891958, 12.22828515855315068 ) ) ;
#9235 = CARTESIAN_POINT ( 'NONE',  ( 9.756007997868694659, 63.79342300382748476, -9.331417668431956969 ) ) ;
#9236 = CARTESIAN_POINT ( 'NONE',  ( 8.258744052426084892, 42.86546257631440682, -10.67932141422061321 ) ) ;
#9237 = CARTESIAN_POINT ( 'NONE',  ( 13.48370246411360007, 39.45286182076745973, -0.6632466905270354429 ) ) ;
#9238 = EDGE_LOOP ( 'NONE', ( #12149, #12154 ) ) ;
#9239 = CARTESIAN_POINT ( 'NONE',  ( -5.218516266495215383, 70.36866619998554029, -12.45060025241497392 ) ) ;
#9240 = CARTESIAN_POINT ( 'NONE',  ( -11.01488299834593398, 61.63543230260535211, -7.805738559095912521 ) ) ;
#9241 = VECTOR ( 'NONE', #7202, 999.9999999999998863 ) ;
#9242 = CARTESIAN_POINT ( 'NONE',  ( -7.409984580736203970E-16, 1.680000000000003491, 12.37355403259654985 ) ) ;
#9243 = ORIENTED_EDGE ( 'NONE', *, *, #2187, .F. ) ;
#9244 = ORIENTED_EDGE ( 'NONE', *, *, #1955, .F. ) ;
#9245 = CARTESIAN_POINT ( 'NONE',  ( 13.49999999999999822, 27.28000000000000469, 4.386415899144237684 ) ) ;
#9246 = CARTESIAN_POINT ( 'NONE',  ( -13.16986379960055231, -43.70624999999989768, 13.16986379959834252 ) ) ;
#9247 = CARTESIAN_POINT ( 'NONE',  ( 4.358999193701488473, 47.83663064582479763, 12.78017842383276026 ) ) ;
#9248 = CARTESIAN_POINT ( 'NONE',  ( 17.42428528562858148, 5.918584287042170544, -19.29752010712846300 ) ) ;
#9249 = CARTESIAN_POINT ( 'NONE',  ( 13.44867813269597256, 57.47128097947902603, -1.193486346532614650 ) ) ;
#9250 = CARTESIAN_POINT ( 'NONE',  ( 9.520470885617715595, 67.12999999999999545, 6.917026985038134512 ) ) ;
#9251 = CARTESIAN_POINT ( 'NONE',  ( 9.520470885617715595, 79.13000000000000966, 6.917026985038134512 ) ) ;
#9252 = CARTESIAN_POINT ( 'NONE',  ( -0.7509811273915951713, 47.65300835411569835, 13.47975592905208408 ) ) ;
#9253 = DIRECTION ( 'NONE',  ( -0.000000000000000000, 1.000000000000000000, -0.000000000000000000 ) ) ;
#9254 = CARTESIAN_POINT ( 'NONE',  ( -8.343458848123578520, 33.47999999999999687, -11.48378591275254124 ) ) ;
#9255 = CARTESIAN_POINT ( 'NONE',  ( 9.538709233711902776E-13, -20.81249999999995026, -11.37500000000000000 ) ) ;
#9256 = CARTESIAN_POINT ( 'NONE',  ( 10.92172942406179104, 44.72999999999999687, -7.935100905948385908 ) ) ;
#9257 = CARTESIAN_POINT ( 'NONE',  ( 8.279083854085270033, 33.86453316571641636, -10.66335730974682328 ) ) ;
#9258 = CARTESIAN_POINT ( 'NONE',  ( -4.923806175756706871, 73.35756458033155525, -12.57016591232264346 ) ) ;
#9259 = VERTEX_POINT ( 'NONE', #10977 ) ;
#9260 = ADVANCED_FACE ( 'NONE', ( #11396 ), #275, .F. ) ;
#9261 = EDGE_LOOP ( 'NONE', ( #9958, #12047, #6166, #11677 ) ) ;
#9262 = CARTESIAN_POINT ( 'NONE',  ( 2.272985001014427393E-15, 74.17999999999997840, -12.37355403259654807 ) ) ;
#9263 = EDGE_LOOP ( 'NONE', ( #10642, #14001, #2064, #11071 ) ) ;
#9264 = CARTESIAN_POINT ( 'NONE',  ( -11.37500000000039613, -83.21562499999981810, 4.711679271993000739 ) ) ;
#9265 = CARTESIAN_POINT ( 'NONE',  ( -0.8503698499406177058, 44.64942536108538462, 13.47335349894747836 ) ) ;
#9266 = CARTESIAN_POINT ( 'NONE',  ( 9.319033143235019523, 8.055054230040793684, 15.43183772185606806 ) ) ;
#9267 = CARTESIAN_POINT ( 'NONE',  ( 11.70509909484535704, 66.68006203444943480, -6.726482417485054377 ) ) ;
#9268 = CARTESIAN_POINT ( 'NONE',  ( 13.49999999999999822, 42.27999999999998693, 4.386415899144237684 ) ) ;
#9269 = CARTESIAN_POINT ( 'NONE',  ( -8.444600773403701410, 71.35698679582962711, 10.53374541731779779 ) ) ;
#9270 = CARTESIAN_POINT ( 'NONE',  ( -13.16986379959834252, 1.006250000000015854, -13.16986379960055409 ) ) ;
#9271 = CARTESIAN_POINT ( 'NONE',  ( -11.67156957293478392, 68.18230872327396241, 6.784133325023568695 ) ) ;
#9272 = CARTESIAN_POINT ( 'NONE',  ( -13.16986379959834252, -15.64374999999994387, -13.16986379960055409 ) ) ;
#9273 = CARTESIAN_POINT ( 'NONE',  ( 9.383209111987648399, 54.81214344578170028, -9.706371691115846190 ) ) ;
#9274 = CARTESIAN_POINT ( 'NONE',  ( -7.272992578804310604, 19.38000000000000256, 10.01041549318726709 ) ) ;
#9275 = CARTESIAN_POINT ( 'NONE',  ( -18.62499999999934985, -73.88437499999982094, -7.714727599200458918 ) ) ;
#9276 = CARTESIAN_POINT ( 'NONE',  ( -12.69097448754075153, 65.09640307793360137, 4.603221522599070248 ) ) ;
#9277 = EDGE_CURVE ( 'NONE', #15564, #17188, #605, .T. ) ;
#9278 = CARTESIAN_POINT ( 'NONE',  ( -0.4450007729775921073, 35.66413109349914379, 13.50000000012882673 ) ) ;
#9279 = CARTESIAN_POINT ( 'NONE',  ( -10.92172942406179104, 18.22999999999999687, 7.935100905948385908 ) ) ;
#9280 = ORIENTED_EDGE ( 'NONE', *, *, #5806, .T. ) ;
#9281 = DIRECTION ( 'NONE',  ( 0.000000000000000000, -1.000000000000000000, 0.000000000000000000 ) ) ;
#9282 = CARTESIAN_POINT ( 'NONE',  ( -11.76794919243112325, 27.78000000000000114, -3.823638476888998827 ) ) ;
#9283 = CARTESIAN_POINT ( 'NONE',  ( -10.15792449496252559, 31.58756608837766322, -8.891980599737237867 ) ) ;
#9284 = PLANE ( 'NONE',  #12477 ) ;
#9285 = CARTESIAN_POINT ( 'NONE',  ( 10.66606376283899849, 60.11536726588247603, 8.275573716453372697 ) ) ;
#9286 = CARTESIAN_POINT ( 'NONE',  ( -4.171729424061791036, -8.469999999999998863, 12.83926296998457239 ) ) ;
#9287 = CARTESIAN_POINT ( 'NONE',  ( -11.05063697790893151, 53.22239444724469593, 7.754578906011509787 ) ) ;
#9288 = CARTESIAN_POINT ( 'NONE',  ( 11.76794919243112325, 43.42999999999999972, 1.441158131103945434E-15 ) ) ;
#9289 = CARTESIAN_POINT ( 'NONE',  ( 8.343458848123578520, 70.98000000000000398, 11.48378591275254124 ) ) ;
#9290 = CARTESIAN_POINT ( 'NONE',  ( 4.989694493860166169, 50.86003338036692156, 12.54404222780582678 ) ) ;
#9291 = VECTOR ( 'NONE', #2872, 1000.000000000000000 ) ;
#9292 = CARTESIAN_POINT ( 'NONE',  ( -11.87437356564380231, 37.69230843674236553, -6.422561873346305461 ) ) ;
#9293 = CARTESIAN_POINT ( 'NONE',  ( 9.155631919984074329, 36.03665308525259547, 9.921063363676065450 ) ) ;
#9294 = CARTESIAN_POINT ( 'NONE',  ( 11.37499999999960210, -89.45937499999983800, 4.711679271994916540 ) ) ;
#9295 = CARTESIAN_POINT ( 'NONE',  ( -5.934342680240685119, 74.46365109743285871, 12.12580240077073412 ) ) ;
#9296 =( BOUNDED_CURVE ( )  B_SPLINE_CURVE ( 2, ( #8247, #12035, #2729, #5412, #10801, #9488, #4253, #15013, #8157, #2904, #13521, #10629, #1411 ),
 .UNSPECIFIED., .F., .F. ) 
 B_SPLINE_CURVE_WITH_KNOTS ( ( 3, 2, 2, 2, 2, 2, 3 ),
 ( 0.4583333333333333148, 0.4611111111111111382, 0.4666666666666666741, 0.4722222222222222099, 0.4777777777777778012, 0.4833333333333333370, 0.4861111111111111049 ),
 .UNSPECIFIED. ) 
 CURVE ( )  GEOMETRIC_REPRESENTATION_ITEM ( )  RATIONAL_B_SPLINE_CURVE ( ( 0.9755282581475768211, 0.9755282581475765991, 1.000000000000000000, 0.9510565162951535312, 1.000000000000000000, 0.9510565162951535312, 1.000000000000000000, 0.9510565162951535312, 1.000000000000000000, 0.9510565162951535312, 1.000000000000000000, 0.9755282581475768211, 0.9755282581475768211 ) ) 
 REPRESENTATION_ITEM ( '' )  );
#9297 = CARTESIAN_POINT ( 'NONE',  ( -13.39208215449344941, 76.99130208596071157, 1.760095884909723685 ) ) ;
#9298 = ADVANCED_FACE ( 'NONE', ( #9663 ), #3427, .T. ) ;
#9299 = CARTESIAN_POINT ( 'NONE',  ( -12.09599699536484074, 80.15074345234548048, 5.999183590577513492 ) ) ;
#9300 = CARTESIAN_POINT ( 'NONE',  ( -7.409984580736203970E-16, 13.67999999999999616, 12.37355403259654985 ) ) ;
#9301 = DIRECTION ( 'NONE',  ( 0.000000000000000000, 1.000000000000000000, 0.000000000000000000 ) ) ;
#9302 = CARTESIAN_POINT ( 'NONE',  ( 11.76794919243112325, 2.430000000000015703, 1.734723475976807094E-15 ) ) ;
#9303 = CARTESIAN_POINT ( 'NONE',  ( 11.76794919243112680, 52.57999999999999829, -3.823638476888993942 ) ) ;
#9304 = CARTESIAN_POINT ( 'NONE',  ( 11.37500000000039613, -60.39062499999985079, -4.711679271993004292 ) ) ;
#9305 = CARTESIAN_POINT ( 'NONE',  ( 7.999999999999904965, 0.000000000000000000, 17.32050807568881368 ) ) ;
#9306 = CARTESIAN_POINT ( 'NONE',  ( 8.343458848123583849, -11.12000000000000632, -11.48378591275253768 ) ) ;
#9307 = CARTESIAN_POINT ( 'NONE',  ( -2.522983078673279752E-14, 34.17999999999999972, -13.50000000000000000 ) ) ;
#9308 = CARTESIAN_POINT ( 'NONE',  ( 6.211406753928388369, 75.95263760063524217, -11.98618433922874971 ) ) ;
#9309 = AXIS2_PLACEMENT_3D ( 'NONE', #3570, #7834, #11714 ) ;
#9310 = CARTESIAN_POINT ( 'NONE',  ( 0.000000000000000000, 80.93000000000000682, 0.000000000000000000 ) ) ;
#9311 = CARTESIAN_POINT ( 'NONE',  ( 3.636496289402154414, 36.82999999999999119, 11.19198476289190936 ) ) ;
#9312 = CARTESIAN_POINT ( 'NONE',  ( -8.891200544363830713E-16, 52.67999999999999972, 13.50000000000000000 ) ) ;
#9313 = CARTESIAN_POINT ( 'NONE',  ( -11.18802534011951089, 58.64595677209553060, -7.555005769838619045 ) ) ;
#9314 = CARTESIAN_POINT ( 'NONE',  ( 2.733029698975450561, 44.77825814313435160, 13.22063484719044446 ) ) ;
#9315 = CARTESIAN_POINT ( 'NONE',  ( 11.44248451431741920, 69.69823784285739521, -7.175533620089728615 ) ) ;
#9316 = CARTESIAN_POINT ( 'NONE',  ( 19.29752010712840615, 5.918584287042170544, 17.42428528562864898 ) ) ;
#9317 = CARTESIAN_POINT ( 'NONE',  ( 8.003658781154468826, 29.98262411852719467, 10.89684441794628178 ) ) ;
#9318 = VECTOR ( 'NONE', #3597, 999.9999999999998863 ) ;
#9319 = CARTESIAN_POINT ( 'NONE',  ( -7.425056585661820918, 55.45770273588824040, -11.27470554016973558 ) ) ;
#9320 = CARTESIAN_POINT ( 'NONE',  ( -10.98422049107948162, 50.22634674789875930, 7.848442420211892312 ) ) ;
#9321 = CARTESIAN_POINT ( 'NONE',  ( 13.13202905021172739, 63.54286607046783075, -3.179279687117263720 ) ) ;
#9322 = CARTESIAN_POINT ( 'NONE',  ( 9.030750244556848827, 42.82969952195247032, -10.04841296085617408 ) ) ;
#9323 = CARTESIAN_POINT ( 'NONE',  ( 13.31381771166605610, 39.35152470227890120, 2.234341475219394191 ) ) ;
#9324 = ORIENTED_EDGE ( 'NONE', *, *, #4456, .T. ) ;
#9325 = CARTESIAN_POINT ( 'NONE',  ( -9.869436736026338863, 70.57243612470094263, -9.211103986266559573 ) ) ;
#9326 = CARTESIAN_POINT ( 'NONE',  ( -4.711679271993003404, -5.203124999999986677, -11.37500000000039435 ) ) ;
#9327 = CARTESIAN_POINT ( 'NONE',  ( -11.76794919243112325, 1.080000000000000959, 3.823638476888994386 ) ) ;
#9328 = VERTEX_POINT ( 'NONE', #2905 ) ;
#9329 = ORIENTED_EDGE ( 'NONE', *, *, #10408, .F. ) ;
#9330 = CARTESIAN_POINT ( 'NONE',  ( -10.92172942406179104, 23.23000000000000043, 7.935100905948385908 ) ) ;
#9331 = DIRECTION ( 'NONE',  ( 0.000000000000000000, 0.000000000000000000, -1.000000000000000000 ) ) ;
#9332 = CARTESIAN_POINT ( 'NONE',  ( 0.5926867827603224947, 61.15868919920450963, -13.50000000000000533 ) ) ;
#9333 = CARTESIAN_POINT ( 'NONE',  ( -4.171729424061791036, 15.53000000000001535, 12.83926296998457239 ) ) ;
#9334 = CARTESIAN_POINT ( 'NONE',  ( 5.868303365318634057, 71.89333723728957182, 12.18994050556831432 ) ) ;
#9335 = CARTESIAN_POINT ( 'NONE',  ( 12.27816310394378618, 57.22451155556443325, 5.613071804343426230 ) ) ;
#9336 = CARTESIAN_POINT ( 'NONE',  ( -9.520470885617715595, 71.62999999999999545, -6.917026985038136289 ) ) ;
#9337 = CARTESIAN_POINT ( 'NONE',  ( 11.76794919243112325, 73.27999999999998693, 3.823638476888996607 ) ) ;
#9338 = CARTESIAN_POINT ( 'NONE',  ( -7.135169524617141157, 47.41465332180884928, 11.46036377623952518 ) ) ;
#9339 = EDGE_CURVE ( 'NONE', #9499, #3828, #9002, .T. ) ;
#9340 = CARTESIAN_POINT ( 'NONE',  ( 1.653273178848926472E-15, 80.93000000000000682, 13.50000000000000000 ) ) ;
#9341 = CARTESIAN_POINT ( 'NONE',  ( 4.790739404487174724, -100.0000000000000000, 15.33879092982343195 ) ) ;
#9342 = LINE ( 'NONE', #10739, #6009 ) ;
#9343 = CARTESIAN_POINT ( 'NONE',  ( 8.043339635996302306, -73.91874999999977547, 8.043339635997654113 ) ) ;
#9344 = CARTESIAN_POINT ( 'NONE',  ( -10.92957602604999146, 9.999999999999998224, 4.954227274842499362 ) ) ;
#9345 = CARTESIAN_POINT ( 'NONE',  ( 12.00008335267889770, 33.65815378040278461, -6.184496803329829540 ) ) ;
#9346 = CARTESIAN_POINT ( 'NONE',  ( -2.171953792510105785, 73.25809419849412052, -13.32423682163636158 ) ) ;
#9347 = ORIENTED_EDGE ( 'NONE', *, *, #16652, .T. ) ;
#9348 = ORIENTED_EDGE ( 'NONE', *, *, #7977, .T. ) ;
#9349 = CARTESIAN_POINT ( 'NONE',  ( 7.272992578804311492, 76.88000000000000966, -10.01041549318726886 ) ) ;
#9350 = ORIENTED_EDGE ( 'NONE', *, *, #10230, .F. ) ;
#9351 = CARTESIAN_POINT ( 'NONE',  ( -11.37500000000039613, -49.91562499999989910, 4.711679271993000739 ) ) ;
#9352 = CARTESIAN_POINT ( 'NONE',  ( -10.23448921847879767, 44.26842627805543628, 8.804069348283245944 ) ) ;
#9353 = CARTESIAN_POINT ( 'NONE',  ( -7.499999999999995559, -27.73865070282584355, 2.034160311361949525 ) ) ;
#9354 = CARTESIAN_POINT ( 'NONE',  ( -13.49999999999999822, 41.07999999999999119, 4.386415899144235908 ) ) ;
#9355 = CARTESIAN_POINT ( 'NONE',  ( -11.85829282994047951, 71.16891807040060769, 6.452231282962286762 ) ) ;
#9356 = EDGE_CURVE ( 'NONE', #2325, #7575, #134, .T. ) ;
#9357 = CARTESIAN_POINT ( 'NONE',  ( 13.16986379959833897, -57.26874999999984794, 13.16986379960055409 ) ) ;
#9358 = CARTESIAN_POINT ( 'NONE',  ( -13.42977164799404477, 67.97782640706279267, 1.375757549377632616 ) ) ;
#9359 = CARTESIAN_POINT ( 'NONE',  ( 7.714727599197340524, -6.278124999999967315, 18.62500000000063949 ) ) ;
#9360 = DIRECTION ( 'NONE',  ( 0.000000000000000000, 0.000000000000000000, 1.000000000000000000 ) ) ;
#9361 = CARTESIAN_POINT ( 'NONE',  ( 11.76794919243112325, 20.28000000000000824, 3.823638476888996163 ) ) ;
#9362 = CARTESIAN_POINT ( 'NONE',  ( 0.000000000000000000, 5.918584287042170544, 0.000000000000000000 ) ) ;
#9363 = CARTESIAN_POINT ( 'NONE',  ( -13.23299063688473254, 64.83510572243652348, -2.688547527704578055 ) ) ;
#9364 = CARTESIAN_POINT ( 'NONE',  ( -9.394804903059576162, 35.31160530982987211, 9.694722408649251832 ) ) ;
#9365 = VERTEX_POINT ( 'NONE', #6102 ) ;
#9366 = CARTESIAN_POINT ( 'NONE',  ( -3.659578208143946298, 3.720968205702268948E-15, -11.78367615807299806 ) ) ;
#9367 = CARTESIAN_POINT ( 'NONE',  ( -8.048289098797699381, 31.48504910120772493, -10.83861414461898676 ) ) ;
#9368 = CARTESIAN_POINT ( 'NONE',  ( 0.000000000000000000, 0.000000000000000000, 0.000000000000000000 ) ) ;
#9369 = CARTESIAN_POINT ( 'NONE',  ( 7.272992578804311492, -12.12000000000000455, -10.01041549318726709 ) ) ;
#9370 = CARTESIAN_POINT ( 'NONE',  ( 0.6926007647112457644, 59.70487025096267786, 13.50000000000703082 ) ) ;
#9371 = CARTESIAN_POINT ( 'NONE',  ( -10.92172942406179104, -5.769999999999997797, 7.935100905948385908 ) ) ;
#9372 = CARTESIAN_POINT ( 'NONE',  ( -11.47944231658861369, 53.19580613508185962, 7.116485988125050177 ) ) ;
#9373 = CARTESIAN_POINT ( 'NONE',  ( -3.636496289402155746, 51.53000000000000114, 11.19198476289190936 ) ) ;
#9374 = APPLICATION_PROTOCOL_DEFINITION ( 'draft international standard', 'automotive_design', 1998, #13204 ) ;
#9375 = CARTESIAN_POINT ( 'NONE',  ( 8.343458848123578520, 67.98000000000000398, 11.48378591275254124 ) ) ;
#9376 = EDGE_CURVE ( 'NONE', #14883, #39, #12113, .T. ) ;
#9377 = CARTESIAN_POINT ( 'NONE',  ( 12.48943337819306620, 51.24351970055675309, 5.124847635520794142 ) ) ;
#9378 = CARTESIAN_POINT ( 'NONE',  ( -8.085997966447257213, 37.48674016390275199, -10.81050427210594300 ) ) ;
#9379 = CARTESIAN_POINT ( 'NONE',  ( 9.439026618432063032, 36.05056385420601117, 9.652180085524300068 ) ) ;
#9380 = CARTESIAN_POINT ( 'NONE',  ( -7.714727599197334307, -29.10312499999994884, -18.62500000000064659 ) ) ;
#9381 = CARTESIAN_POINT ( 'NONE',  ( -8.677731035997348741, 74.34615417660486969, 10.34231826630725237 ) ) ;
#9382 = CARTESIAN_POINT ( 'NONE',  ( -13.29658185220932332, 76.84789797714496729, -2.334733406331294781 ) ) ;
#9383 = CARTESIAN_POINT ( 'NONE',  ( -8.225013884042102319, 80.36731853247339075, 10.71434597753230911 ) ) ;
#9384 = CARTESIAN_POINT ( 'NONE',  ( 7.499999999999998224, 108.7391404411723528, -0.5315352956498786696 ) ) ;
#9385 = CARTESIAN_POINT ( 'NONE',  ( -13.49999999999999822, 8.079999999999996518, 4.386415899144235020 ) ) ;
#9386 = CARTESIAN_POINT ( 'NONE',  ( 7.272992578804308828, 1.980000000000001315, 10.01041549318726709 ) ) ;
#9387 = CARTESIAN_POINT ( 'NONE',  ( -9.520470885617715595, 44.62999999999999545, -6.917026985038136289 ) ) ;
#9388 = CARTESIAN_POINT ( 'NONE',  ( -11.37500000000000178, -51.02499999999986358, -9.545674412382054647E-13 ) ) ;
#9389 = CARTESIAN_POINT ( 'NONE',  ( -18.62499999999934985, -40.58437499999990905, -7.714727599200458918 ) ) ;
#9390 = CARTESIAN_POINT ( 'NONE',  ( -8.343458848123582072, -9.620000000000002771, 11.48378591275254124 ) ) ;
#9391 = CARTESIAN_POINT ( 'NONE',  ( -11.36904938338338944, 40.65721801956971859, -7.283062199855843133 ) ) ;
#9392 = CIRCLE ( 'NONE', #7693, 5.000000000000000000 ) ;
#9393 = CARTESIAN_POINT ( 'NONE',  ( 0.000000000000000000, 0.000000000000000000, 0.000000000000000000 ) ) ;
#9394 = CARTESIAN_POINT ( 'NONE',  ( 12.66318051525177601, 75.60094073508014390, -4.729132707123133272 ) ) ;
#9395 = CARTESIAN_POINT ( 'NONE',  ( 8.343458848123580296, 67.98000000000000398, 11.48378591275253768 ) ) ;
#9396 = CARTESIAN_POINT ( 'NONE',  ( 4.171729424061791924, 51.03000000000000114, -12.83926296998457239 ) ) ;
#9397 = CARTESIAN_POINT ( 'NONE',  ( 11.76794919243112680, 43.57999999999999119, -3.823638476888993942 ) ) ;
#9398 = CARTESIAN_POINT ( 'NONE',  ( -8.657037944518233274, 41.34728218387066789, 10.36125059353578948 ) ) ;
#9399 = EDGE_CURVE ( 'NONE', #368, #9696, #7506, .T. ) ;
#9400 = CARTESIAN_POINT ( 'NONE',  ( -12.77783441696706035, 58.77300612785465006, -4.356290537409963193 ) ) ;
#9401 = CARTESIAN_POINT ( 'NONE',  ( 4.678274206804918123, 44.84844931136031221, 12.66349204453718968 ) ) ;
#9402 = VECTOR ( 'NONE', #5988, 999.9999999999998863 ) ;
#9403 = CARTESIAN_POINT ( 'NONE',  ( -4.171729424061791036, 55.52999999999999403, 12.83926296998457239 ) ) ;
#9404 = CARTESIAN_POINT ( 'NONE',  ( 10.38497083786669428, 30.09949477856799760, 8.633462984270375173 ) ) ;
#9405 = CARTESIAN_POINT ( 'NONE',  ( -10.71735289789100420, 55.61806186037063071, -8.210225439848542806 ) ) ;
#9406 = CARTESIAN_POINT ( 'NONE',  ( -11.21169442594827892, 49.64742185618261772, -7.519853369252744280 ) ) ;
#9407 = CARTESIAN_POINT ( 'NONE',  ( 12.87829787502431245, 63.57557519788824152, -4.054628780689018441 ) ) ;
#9408 = CARTESIAN_POINT ( 'NONE',  ( 11.92131337477997732, 42.66417587640939502, -6.335005369018095855 ) ) ;
#9409 = CARTESIAN_POINT ( 'NONE',  ( 9.285075054945489015, 39.04297856348830464, 9.799891255916394428 ) ) ;
#9410 = ORIENTED_EDGE ( 'NONE', *, *, #640, .F. ) ;
#9411 = CARTESIAN_POINT ( 'NONE',  ( -7.756731982646783763, 70.47211894010109745, -11.04912417935179647 ) ) ;
#9412 = CARTESIAN_POINT ( 'NONE',  ( -5.281055406448098636E-10, 61.18000001472334759, -13.50000000000000000 ) ) ;
#9413 = ORIENTED_EDGE ( 'NONE', *, *, #16937, .T. ) ;
#9414 = ORIENTED_EDGE ( 'NONE', *, *, #7659, .F. ) ;
#9415 = CARTESIAN_POINT ( 'NONE',  ( -13.49999999999999822, 19.78000000000000824, -4.386415899144240349 ) ) ;
#9416 = CARTESIAN_POINT ( 'NONE',  ( -7.714727599200467800, -44.74687499999989626, 18.62499999999934630 ) ) ;
#9417 = CARTESIAN_POINT ( 'NONE',  ( 6.605773061280451941, 47.92331672993605451, 11.77343924215295345 ) ) ;
#9418 = CARTESIAN_POINT ( 'NONE',  ( -13.49999999999999822, 12.08000000000000185, 4.386415899144235908 ) ) ;
#9419 = AXIS2_PLACEMENT_3D ( 'NONE', #14476, #11934, #2539 ) ;
#9420 = CARTESIAN_POINT ( 'NONE',  ( 9.811143588542840632, 72.06941418877464400, 9.273190923045845580 ) ) ;
#9421 = CARTESIAN_POINT ( 'NONE',  ( 12.38238512554978499, 57.62633858785935814, -5.378349744821834477 ) ) ;
#9422 = CARTESIAN_POINT ( 'NONE',  ( -7.272992578804307939, 71.48000000000000398, -10.01041549318726886 ) ) ;
#9423 = CARTESIAN_POINT ( 'NONE',  ( -7.576616670048093940E-16, 72.68000000000000682, 12.37355403259654985 ) ) ;
#9424 = CARTESIAN_POINT ( 'NONE',  ( -7.098413309481311551, 47.41620383881762990, 11.48314148660388767 ) ) ;
#9425 = LINE ( 'NONE', #9340, #16609 ) ;
#9426 = CARTESIAN_POINT ( 'NONE',  ( 2.445080149700053643E-15, 39.17999999999999972, -13.50000000000000000 ) ) ;
#9427 = CARTESIAN_POINT ( 'NONE',  ( -4.171729424061787483, 33.32999999999999829, -12.83926296998457417 ) ) ;
#9428 = CARTESIAN_POINT ( 'NONE',  ( 8.043339635997654113, -35.38124999999991616, -8.043339635996304082 ) ) ;
#9429 = CARTESIAN_POINT ( 'NONE',  ( -8.891200544363830713E-16, 52.67999999999999972, 13.50000000000000000 ) ) ;
#9430 = CARTESIAN_POINT ( 'NONE',  ( 11.89722853480184028, 33.66600382463642660, -6.380526270711741610 ) ) ;
#9431 = CARTESIAN_POINT ( 'NONE',  ( -9.624821359540113974, 73.55990925749743781, -9.466443300615020817 ) ) ;
#9432 = ORIENTED_EDGE ( 'NONE', *, *, #4773, .F. ) ;
#9433 = VERTEX_POINT ( 'NONE', #776 ) ;
#9434 = CARTESIAN_POINT ( 'NONE',  ( -3.636496289402155746, 72.53000000000000114, 11.19198476289190936 ) ) ;
#9435 = VERTEX_POINT ( 'NONE', #6182 ) ;
#9436 = CARTESIAN_POINT ( 'NONE',  ( -13.32261196877928455, 41.00656928112289279, 2.181370886427688394 ) ) ;
#9437 = CARTESIAN_POINT ( 'NONE',  ( -4.711679271993001628, -95.70312499999977263, -11.37500000000039613 ) ) ;
#9438 = EDGE_CURVE ( 'NONE', #16090, #3801, #7620, .T. ) ;
#9439 = CARTESIAN_POINT ( 'NONE',  ( -10.12145965770221245, 44.27437845011841233, 8.933423452156974420 ) ) ;
#9440 = CARTESIAN_POINT ( 'NONE',  ( 8.111079018422898912, 7.924936010579560097, 16.64104048077467013 ) ) ;
#9441 = CARTESIAN_POINT ( 'NONE',  ( 10.92172942406179104, 39.72999999999999687, -7.935100905948385908 ) ) ;
#9442 = CARTESIAN_POINT ( 'NONE',  ( -13.45001587941835197, 70.97025115243951632, 1.160810400985216484 ) ) ;
#9443 = CARTESIAN_POINT ( 'NONE',  ( 18.62499999999935341, -25.00937499999992397, 7.714727599200469577 ) ) ;
#9444 = CARTESIAN_POINT ( 'NONE',  ( -12.56865293787816462, 67.75091737192668973, -4.934974244349399797 ) ) ;
#9445 = CARTESIAN_POINT ( 'NONE',  ( -18.62500000000064659, -2.115624999999976996, 7.714727599197333419 ) ) ;
#9446 = CARTESIAN_POINT ( 'NONE',  ( 11.65835260217848912, 54.68333460578584493, -6.808186811182635800 ) ) ;
#9447 = CARTESIAN_POINT ( 'NONE',  ( 9.520470885617717371, 17.72999999999999687, -6.917026985038131848 ) ) ;
#9448 = CARTESIAN_POINT ( 'NONE',  ( -1.564113515457998572E-12, -95.73749999999976978, 18.62500000000000000 ) ) ;
#9449 = CARTESIAN_POINT ( 'NONE',  ( -12.43543891747863839, 65.12177667763330646, 5.262208274864947910 ) ) ;
#9450 = CARTESIAN_POINT ( 'NONE',  ( -13.47176300034568541, 34.89984414028458559, -0.8728053654163654418 ) ) ;
#9451 = EDGE_LOOP ( 'NONE', ( #970, #8548 ) ) ;
#9452 = CARTESIAN_POINT ( 'NONE',  ( -10.78033876856473228, 1.259542957514470777E-16, -7.094692149502226819 ) ) ;
#9453 = CARTESIAN_POINT ( 'NONE',  ( -8.891200544363830713E-16, 79.67999999999999261, 13.50000000000000000 ) ) ;
#9454 = CARTESIAN_POINT ( 'NONE',  ( -0.5734647119475105859, 31.20060767735286333, -13.49031509358949243 ) ) ;
#9455 = CARTESIAN_POINT ( 'NONE',  ( 5.953140201857509695, 72.96290519792380280, -12.11652618179868668 ) ) ;
#9456 = CARTESIAN_POINT ( 'NONE',  ( 9.520470885617717371, -12.26999999999999602, -6.917026985038131848 ) ) ;
#9457 = CYLINDRICAL_SURFACE ( 'NONE', #3793, 26.00000000000000355 ) ;
#9458 = CARTESIAN_POINT ( 'NONE',  ( 10.92172942406178926, -4.869999999999999218, 7.935100905948385908 ) ) ;
#9459 = CARTESIAN_POINT ( 'NONE',  ( -13.23519524994845042, 53.02388892134538878, 2.661131415613865236 ) ) ;
#9460 = CARTESIAN_POINT ( 'NONE',  ( 9.520470885617717371, 46.73000000000000398, -6.917026985038131848 ) ) ;
#9461 = CARTESIAN_POINT ( 'NONE',  ( 10.55906642891832448, 51.10936410628003301, 8.412101771180822141 ) ) ;
#9462 = PRODUCT_RELATED_PRODUCT_CATEGORY ( 'part', '', ( #2950 ) ) ;
#9463 = CARTESIAN_POINT ( 'NONE',  ( -10.05898634321896346, 37.58241540748306875, -9.004437385054949061 ) ) ;
#9464 = AXIS2_PLACEMENT_3D ( 'NONE', #13202, #1001, #10479 ) ;
#9465 = CARTESIAN_POINT ( 'NONE',  ( 9.790434661910198955, 36.06810143375782474, 9.303453747971381915 ) ) ;
#9466 = CARTESIAN_POINT ( 'NONE',  ( 13.16986379959833897, -21.81874999999996589, 13.16986379960055409 ) ) ;
#9467 = CARTESIAN_POINT ( 'NONE',  ( -12.00341789873817255, 74.15789563195407652, 6.178041647018932991 ) ) ;
#9468 = CARTESIAN_POINT ( 'NONE',  ( -11.21206813385310852, 76.64744563254819809, -7.519279139868476847 ) ) ;
#9469 = CARTESIAN_POINT ( 'NONE',  ( -12.42682143791030747, 80.12235603135506778, 5.276029534630485962 ) ) ;
#9470 = CARTESIAN_POINT ( 'NONE',  ( -9.520470885617715595, 12.63000000000000256, -6.917026985038136289 ) ) ;
#9471 = CARTESIAN_POINT ( 'NONE',  ( -4.886222543809949137, 80.93000000000003524, 11.77926528190478095 ) ) ;
#9472 = CARTESIAN_POINT ( 'NONE',  ( -8.891200544363830713E-16, 8.679999999999999716, 13.49999999999999822 ) ) ;
#9473 = CARTESIAN_POINT ( 'NONE',  ( -3.636496289402152637, 6.330000000000001847, -11.19198476289190936 ) ) ;
#9474 = EDGE_CURVE ( 'NONE', #2562, #17099, #5643, .T. ) ;
#9475 = CARTESIAN_POINT ( 'NONE',  ( 7.272992578804308828, 45.97999999999999687, 10.01041549318726886 ) ) ;
#9476 = CARTESIAN_POINT ( 'NONE',  ( 4.711679271994909435, -53.07187499999987068, -11.37499999999960387 ) ) ;
#9477 = DIRECTION ( 'NONE',  ( -7.483177508809139424E-15, 0.000000000000000000, 1.000000000000000000 ) ) ;
#9478 = CARTESIAN_POINT ( 'NONE',  ( -13.49999999999999822, -4.219999999999998863, -4.386415899144240349 ) ) ;
#9479 = ADVANCED_FACE ( 'NONE', ( #6920 ), #12297, .F. ) ;
#9480 = CARTESIAN_POINT ( 'NONE',  ( -8.140112397462228699, 40.48917452635999581, -10.76980339117528196 ) ) ;
#9481 = CARTESIAN_POINT ( 'NONE',  ( 2.445080149700053643E-15, 36.17999999999999972, -13.50000000000000000 ) ) ;
#9482 = CARTESIAN_POINT ( 'NONE',  ( 11.26111035850912145, 75.15046918880804583, 7.446692750201517441 ) ) ;
#9483 = CARTESIAN_POINT ( 'NONE',  ( 0.000000000000000000, 30.93000000000001393, 0.000000000000000000 ) ) ;
#9484 = CARTESIAN_POINT ( 'NONE',  ( -7.272992578804307939, 41.47999999999999687, -10.01041549318726886 ) ) ;
#9485 = CARTESIAN_POINT ( 'NONE',  ( -11.19689435447929071, 41.21349520832467306, 7.541861633535862808 ) ) ;
#9486 = CARTESIAN_POINT ( 'NONE',  ( -9.286707789763200438, 58.54294910056232482, -9.800380398344652022 ) ) ;
#9487 = CARTESIAN_POINT ( 'NONE',  ( -1.900613283894451611, 9.122906826104705047, -11.99999999999999645 ) ) ;
#9488 = CARTESIAN_POINT ( 'NONE',  ( 13.50000000000000355, 59.57999999999999829, -4.386415899144233244 ) ) ;
#9489 = CARTESIAN_POINT ( 'NONE',  ( 11.06245251677889740, 30.13829864597929742, 7.738284462911099837 ) ) ;
#9490 = LINE ( 'NONE', #2994, #623 ) ;
#9491 = CARTESIAN_POINT ( 'NONE',  ( -12.08639118943488455, 49.70860411622489750, -6.014117973902937564 ) ) ;
#9492 = CARTESIAN_POINT ( 'NONE',  ( 13.49574338918140626, 63.41592130795832816, 0.4033985791695099965 ) ) ;
#9493 = CARTESIAN_POINT ( 'NONE',  ( 12.94155513399510404, 42.56773774999591353, -3.846463401272276261 ) ) ;
#9494 = CARTESIAN_POINT ( 'NONE',  ( -18.36027427702395798, 7.956016705491392393, 1.158215859972792527 ) ) ;
#9495 = EDGE_LOOP ( 'NONE', ( #3000, #325, #8647, #9194 ) ) ;
#9496 = CARTESIAN_POINT ( 'NONE',  ( 2.138189944381242213, 75.10311857767970878, -13.49999999999999822 ) ) ;
#9497 = CARTESIAN_POINT ( 'NONE',  ( -8.891200544363830713E-16, 49.67999999999999261, 13.50000000000000000 ) ) ;
#9498 = CARTESIAN_POINT ( 'NONE',  ( 8.343458848123578520, 11.98000000000000753, 11.48378591275254124 ) ) ;
#9499 = VERTEX_POINT ( 'NONE', #6352 ) ;
#9500 = EDGE_CURVE ( 'NONE', #2957, #7801, #16053, .T. ) ;
#9501 = CARTESIAN_POINT ( 'NONE',  ( -5.427788510536279531, 43.37664531000118728, -12.36142337679662973 ) ) ;
#9502 = CARTESIAN_POINT ( 'NONE',  ( 18.62499999999934630, -48.90937499999989058, 7.714727599200467800 ) ) ;
#9503 = CARTESIAN_POINT ( 'NONE',  ( 10.10993224895466369, 60.77529409556134965, -8.962226066154812543 ) ) ;
#9504 = AXIS2_PLACEMENT_3D ( 'NONE', #10870, #16239, #4148 ) ;
#9505 = CARTESIAN_POINT ( 'NONE',  ( -4.171729424061787483, 14.33000000000000895, -12.83926296998457417 ) ) ;
#9506 = DIRECTION ( 'NONE',  ( 0.000000000000000000, 1.000000000000000000, 0.000000000000000000 ) ) ;
#9507 = CARTESIAN_POINT ( 'NONE',  ( 12.39353830234175824, 57.62533442192442834, -5.352606972886608361 ) ) ;
#9508 = CARTESIAN_POINT ( 'NONE',  ( -7.576616670048093940E-16, 66.67999999999997840, 12.37355403259654985 ) ) ;
#9509 = CARTESIAN_POINT ( 'NONE',  ( 2.272985001014427788E-15, 77.18000000000000682, -12.37355403259654985 ) ) ;
#9510 = CARTESIAN_POINT ( 'NONE',  ( -3.807942577807816420, 47.54308049960635429, 12.95182113153237502 ) ) ;
#9511 = DIRECTION ( 'NONE',  ( 0.000000000000000000, 1.000000000000000000, 0.000000000000000000 ) ) ;
#9512 = CARTESIAN_POINT ( 'NONE',  ( 13.50000000000000355, 74.58000000000001251, -4.386415899144233244 ) ) ;
#9513 = CARTESIAN_POINT ( 'NONE',  ( 25.42428528562852819, 0.000000000000000000, 5.441113646577569796 ) ) ;
#9514 = CARTESIAN_POINT ( 'NONE',  ( -9.653558740436345431, 10.00000000000000355, -7.932758269264289730 ) ) ;
#9515 = CARTESIAN_POINT ( 'NONE',  ( -8.043339635997654113, -69.75624999999980957, 8.043339635996304082 ) ) ;
#9516 = VECTOR ( 'NONE', #13950, 1000.000000000000000 ) ;
#9517 = CARTESIAN_POINT ( 'NONE',  ( 4.171729424061789260, 5.830000000000001847, 12.83926296998457239 ) ) ;
#9518 = CARTESIAN_POINT ( 'NONE',  ( 11.23618775536431436, 33.71102971822809025, -7.483199226156876271 ) ) ;
#9519 = CARTESIAN_POINT ( 'NONE',  ( -2.604932354848102261, 73.27367133763648610, -13.24695926549161129 ) ) ;
#9520 = DIRECTION ( 'NONE',  ( -0.8660254037844393737, 0.000000000000000000, 0.4999999999999986122 ) ) ;
#9521 = ORIENTED_EDGE ( 'NONE', *, *, #1628, .F. ) ;
#9522 = CARTESIAN_POINT ( 'NONE',  ( -13.49999999999999822, 42.77999999999999403, -4.386415899144240349 ) ) ;
#9523 = ORIENTED_EDGE ( 'NONE', *, *, #206, .F. ) ;
#9524 = EDGE_CURVE ( 'NONE', #12569, #149, #11323, .T. ) ;
#9525 = CARTESIAN_POINT ( 'NONE',  ( -11.37499999999960210, -97.78437499999979821, -4.711679271994911211 ) ) ;
#9526 = CARTESIAN_POINT ( 'NONE',  ( -11.23485739642284464, 44.21114091592843209, 7.485350584702932686 ) ) ;
#9527 = CARTESIAN_POINT ( 'NONE',  ( -7.499999999999994671, -26.29769599445798534, -6.931232109908926020 ) ) ;
#9528 = AXIS2_PLACEMENT_3D ( 'NONE', #11812, #8821, #15496 ) ;
#9529 = CARTESIAN_POINT ( 'NONE',  ( -13.49999999999999822, 44.07999999999999829, 4.386415899144235908 ) ) ;
#9530 = CARTESIAN_POINT ( 'NONE',  ( -8.691771469529815392E-16, 49.67999999999999972, 14.19474002721660355 ) ) ;
#9531 = CARTESIAN_POINT ( 'NONE',  ( -12.73079347874323908, 71.09226311646531826, 4.495458693738632050 ) ) ;
#9532 = CARTESIAN_POINT ( 'NONE',  ( -7.714727599197334307, -14.60312499999994706, -18.62500000000064659 ) ) ;
#9533 = CARTESIAN_POINT ( 'NONE',  ( -13.43160263846500335, 67.88282665543684402, -1.357254972949814897 ) ) ;
#9534 = CARTESIAN_POINT ( 'NONE',  ( -18.62500000000064659, -35.41562499999989200, 7.714727599197333419 ) ) ;
#9535 = CARTESIAN_POINT ( 'NONE',  ( 13.19418465749268599, 54.53154371968964398, -2.869303380193378494 ) ) ;
#9536 = DIRECTION ( 'NONE',  ( 0.000000000000000000, 0.000000000000000000, -1.000000000000000000 ) ) ;
#9537 = CARTESIAN_POINT ( 'NONE',  ( -13.45471606681021015, 64.89176115380030296, -1.105190539164891295 ) ) ;
#9538 = VERTEX_POINT ( 'NONE', #3041 ) ;
#9539 = CARTESIAN_POINT ( 'NONE',  ( -13.47350605204804097, 34.90077836227690966, -0.8454715895919912017 ) ) ;
#9540 = VERTEX_POINT ( 'NONE', #2235 ) ;
#9541 = CARTESIAN_POINT ( 'NONE',  ( 23.28534784291401749, 6.548267719634618622, -4.206197538246383871 ) ) ;
#9542 = CARTESIAN_POINT ( 'NONE',  ( 7.500000000000003553, -22.25602869842713716, 9.367496997597598352 ) ) ;
#9543 = CARTESIAN_POINT ( 'NONE',  ( 8.106489558427483644, 72.87234586791355184, -10.79566516057443337 ) ) ;
#9544 = CARTESIAN_POINT ( 'NONE',  ( 11.76794919243112325, -9.569999999999994955, 1.734723475976807094E-15 ) ) ;
#9545 = CARTESIAN_POINT ( 'NONE',  ( 3.912904983860617136, 59.82044921492690293, 12.92374366791880469 ) ) ;
#9546 = CARTESIAN_POINT ( 'NONE',  ( -4.171729424061791036, -17.46999999999999886, 12.83926296998457239 ) ) ;
#9547 = CARTESIAN_POINT ( 'NONE',  ( -13.49999999999999822, 71.08000000000001251, 4.386415899144235908 ) ) ;
#9548 = CARTESIAN_POINT ( 'NONE',  ( -11.95834195965728242, 52.69827122100793559, -6.277836442959745078 ) ) ;
#9549 = CARTESIAN_POINT ( 'NONE',  ( 7.272992578804308828, 45.98000000000000398, 10.01041549318726709 ) ) ;
#9550 = CARTESIAN_POINT ( 'NONE',  ( -13.49999999999999822, 63.78000000000000114, -4.386415899144240349 ) ) ;
#9551 = CARTESIAN_POINT ( 'NONE',  ( 12.48553484639394462, 51.24315187460019416, 5.134337538193736172 ) ) ;
#9552 = CARTESIAN_POINT ( 'NONE',  ( -8.363913707455445490, 37.49932944145390934, -10.59726195709811947 ) ) ;
#9553 = CARTESIAN_POINT ( 'NONE',  ( 4.181727136617158003, 35.83035942868416868, 12.83601768139505594 ) ) ;
#9554 = CARTESIAN_POINT ( 'NONE',  ( -18.62499999999935341, -31.18437499999994600, -7.714727599200458030 ) ) ;
#9555 = CARTESIAN_POINT ( 'NONE',  ( -13.01412793683608804, 74.05813771021030334, 3.589233157574757360 ) ) ;
#9556 = CARTESIAN_POINT ( 'NONE',  ( -12.78816704283054762, 76.77399786514027369, -4.329514614045784526 ) ) ;
#9557 = CARTESIAN_POINT ( 'NONE',  ( -8.236863458086046919, 79.49291995815075040, -10.73295259625500009 ) ) ;
#9558 = CARTESIAN_POINT ( 'NONE',  ( -25.42428528562860990, 5.918584287042170544, 5.441113646577212748 ) ) ;
#9559 = CARTESIAN_POINT ( 'NONE',  ( 5.896062637424393849, 80.92999999999999261, 12.11648925032670832 ) ) ;
#9560 = FACE_OUTER_BOUND ( 'NONE', #2586, .T. ) ;
#9561 = CARTESIAN_POINT ( 'NONE',  ( 11.76794919243112325, 5.279999999999999361, 3.823638476888996163 ) ) ;
#9562 = CARTESIAN_POINT ( 'NONE',  ( 9.520470885617717371, 43.72999999999999687, -6.917026985038131848 ) ) ;
#9563 = CARTESIAN_POINT ( 'NONE',  ( -18.62500000000000000, -8.324999999999979750, -1.562973063126292555E-12 ) ) ;
#9564 = CARTESIAN_POINT ( 'NONE',  ( -10.92172942406178926, -4.369999999999999218, -7.935100905948389460 ) ) ;
#9565 = CARTESIAN_POINT ( 'NONE',  ( -5.605660797254122585, 40.38350727605969581, -12.28115835899099118 ) ) ;
#9566 = CARTESIAN_POINT ( 'NONE',  ( 6.750022862106050958, 31.26259509543302784, 11.69132975161703492 ) ) ;
#9567 = CARTESIAN_POINT ( 'NONE',  ( 13.06941462424293121, 75.55044996165509019, -3.382384493177171603 ) ) ;
#9568 = CARTESIAN_POINT ( 'NONE',  ( 18.07672611500867532, 1.677322744816967809E-15, -4.362237117369845762 ) ) ;
#9569 = AXIS2_PLACEMENT_3D ( 'NONE', #4486, #1813, #8480 ) ;
#9570 = CARTESIAN_POINT ( 'NONE',  ( 8.050216715958701030, 31.03187307936174832, 8.940658242654158983 ) ) ;
#9571 = CARTESIAN_POINT ( 'NONE',  ( -9.319066580405237943, 41.31534733134024151, 9.767548834432302485 ) ) ;
#9572 = CARTESIAN_POINT ( 'NONE',  ( -12.47057163453939310, 58.74156942395950409, -5.176736132799251600 ) ) ;
#9573 = ADVANCED_FACE ( 'NONE', ( #11807 ), #3842, .F. ) ;
#9574 = CARTESIAN_POINT ( 'NONE',  ( 2.929103925447447132, 44.78531871342022441, 13.17840735884215064 ) ) ;
#9575 = CARTESIAN_POINT ( 'NONE',  ( -13.50000000000000000, 54.92999999999999972, -3.306546357697853733E-15 ) ) ;
#9576 = CARTESIAN_POINT ( 'NONE',  ( 19.00000000000000711, 0.000000000000000000, -1.732050807568807027 ) ) ;
#9577 = CARTESIAN_POINT ( 'NONE',  ( 1.509281292405760415E-13, 1.813974596215571777, 12.00000000000000000 ) ) ;
#9578 = CARTESIAN_POINT ( 'NONE',  ( -12.17504944591498273, 49.71587186443941420, -5.832774803456854507 ) ) ;
#9579 = CARTESIAN_POINT ( 'NONE',  ( 12.94006017376627860, 63.29219168140004825, 3.847937226494118956 ) ) ;
#9580 = CARTESIAN_POINT ( 'NONE',  ( 10.64860572984884790, 42.11438410854437109, 8.298049206624620311 ) ) ;
#9581 = CARTESIAN_POINT ( 'NONE',  ( 4.045770767957217018, 38.82545391565042081, 12.87990362912008990 ) ) ;
#9582 = AXIS2_PLACEMENT_3D ( 'NONE', #12455, #5748, #14992 ) ;
#9583 = VERTEX_POINT ( 'NONE', #10488 ) ;
#9584 = CARTESIAN_POINT ( 'NONE',  ( -1.962467107901933794, 70.25054030898461122, -13.35786085374755849 ) ) ;
#9585 = DIRECTION ( 'NONE',  ( -0.000000000000000000, -1.000000000000000000, -0.000000000000000000 ) ) ;
#9586 = CARTESIAN_POINT ( 'NONE',  ( -4.171729424061791036, 14.53000000000001535, 12.83926296998457239 ) ) ;
#9587 = ORIENTED_EDGE ( 'NONE', *, *, #3408, .F. ) ;
#9588 = CARTESIAN_POINT ( 'NONE',  ( -4.189387794536774123, 43.33065430922783179, -12.83365974533868936 ) ) ;
#9589 = CARTESIAN_POINT ( 'NONE',  ( -7.499999999999999112, 105.3920397463311218, -8.709571264514705646 ) ) ;
#9590 = CARTESIAN_POINT ( 'NONE',  ( 13.00154923021119302, 60.55982641677310596, -3.634527857254126193 ) ) ;
#9591 = CARTESIAN_POINT ( 'NONE',  ( -13.50000000000000000, 11.92999999999999616, -3.469446951953614189E-15 ) ) ;
#9592 = CARTESIAN_POINT ( 'NONE',  ( 1.561832610794586538E-12, -20.81249999999995026, -18.62500000000000000 ) ) ;
#9593 = CARTESIAN_POINT ( 'NONE',  ( 9.959380740143405575, 66.78290531437225752, -9.113807157362280975 ) ) ;
#9594 = CARTESIAN_POINT ( 'NONE',  ( 6.860306926835040287, 56.93364315233684181, 11.63957199842341517 ) ) ;
#9595 = CARTESIAN_POINT ( 'NONE',  ( 2.272985001014427788E-15, 56.17999999999999972, -12.37355403259654985 ) ) ;
#9596 = CARTESIAN_POINT ( 'NONE',  ( -7.272992578804310604, 63.37999999999998835, 10.01041549318726709 ) ) ;
#9597 = CARTESIAN_POINT ( 'NONE',  ( -11.37861599013445257, 47.20202813202893566, 7.264810526584298600 ) ) ;
#9598 = CIRCLE ( 'NONE', #3380, 9.000000000000000000 ) ;
#9599 = CARTESIAN_POINT ( 'NONE',  ( 3.542742451760277689, 46.05382628669764244, -13.14678535250671843 ) ) ;
#9600 = CARTESIAN_POINT ( 'NONE',  ( 0.000000000000000000, 9.000000000000000000, -12.00000000000000178 ) ) ;
#9601 = EDGE_CURVE ( 'NONE', #11528, #16381, #17009, .T. ) ;
#9602 = CARTESIAN_POINT ( 'NONE',  ( 18.62040007950909271, -99.99999999999997158, 0.8650468441352018312 ) ) ;
#9603 = CARTESIAN_POINT ( 'NONE',  ( -11.79534111549779141, 9.999999999999998224, -2.590977554098922386 ) ) ;
#9604 = CARTESIAN_POINT ( 'NONE',  ( -4.711679271994916540, -78.04687499999982947, 11.37499999999960210 ) ) ;
#9605 = CARTESIAN_POINT ( 'NONE',  ( 10.40591568030824732, 33.75906600926769130, -8.600427378247252008 ) ) ;
#9606 = CARTESIAN_POINT ( 'NONE',  ( 0.000000000000000000, 3.000000000000000000, 0.000000000000000000 ) ) ;
#9607 = PLANE ( 'NONE',  #127 ) ;
#9608 = ORIENTED_EDGE ( 'NONE', *, *, #12715, .F. ) ;
#9609 = CARTESIAN_POINT ( 'NONE',  ( -5.591496387441557303, 62.47704092548192278, 12.28760602409226088 ) ) ;
#9610 = ORIENTED_EDGE ( 'NONE', *, *, #1462, .T. ) ;
#9611 = CARTESIAN_POINT ( 'NONE',  ( -13.43504215837644011, 40.88299209765439457, -1.356889373904522245 ) ) ;
#9612 = CARTESIAN_POINT ( 'NONE',  ( -13.16986379960055409, -34.30624999999993463, 13.16986379959834252 ) ) ;
#9613 = VECTOR ( 'NONE', #7017, 1000.000000000000000 ) ;
#9614 = CARTESIAN_POINT ( 'NONE',  ( -12.83028172577782655, 44.08205989162794936, 4.222530735082791864 ) ) ;
#9615 = CARTESIAN_POINT ( 'NONE',  ( -8.022095340454590939, 7.854010772509913529, 16.97734196418684505 ) ) ;
#9616 = CARTESIAN_POINT ( 'NONE',  ( 10.92172942406179104, 42.72999999999999687, -7.935100905948385908 ) ) ;
#9617 = CARTESIAN_POINT ( 'NONE',  ( 10.92172942406178926, 50.13000000000000256, 7.935100905948387684 ) ) ;
#9618 = CARTESIAN_POINT ( 'NONE',  ( -13.49804976266443113, 70.92212470242434108, -0.2296839510666886242 ) ) ;
#9619 = ADVANCED_FACE ( 'NONE', ( #392 ), #1875, .T. ) ;
#9620 = CARTESIAN_POINT ( 'NONE',  ( -1.564113515457998370E-12, -55.18749999999985079, 18.62500000000000000 ) ) ;
#9621 = CARTESIAN_POINT ( 'NONE',  ( -5.522359042343270019, 67.38028659687103072, -12.31888227721426077 ) ) ;
#9622 = CARTESIAN_POINT ( 'NONE',  ( 7.714727599200456254, -79.12187499999980389, -18.62499999999935341 ) ) ;
#9623 = CARTESIAN_POINT ( 'NONE',  ( 11.88709381102925100, 54.19314474854091657, 6.403576458692946005 ) ) ;
#9624 = CARTESIAN_POINT ( 'NONE',  ( -11.87378271711010846, 65.16811738021863221, 6.431528113332499963 ) ) ;
#9625 = ORIENTED_EDGE ( 'NONE', *, *, #8816, .F. ) ;
#9626 = CARTESIAN_POINT ( 'NONE',  ( 2.445080149700053643E-15, 63.17999999999998550, -13.50000000000000000 ) ) ;
#9627 = CARTESIAN_POINT ( 'NONE',  ( -12.50808303647379027, 35.11473487356274603, 5.079913338622167096 ) ) ;
#9628 = VERTEX_POINT ( 'NONE', #10208 ) ;
#9629 = CARTESIAN_POINT ( 'NONE',  ( 13.06764686229368877, 78.55070251195772357, -3.389196011057948876 ) ) ;
#9630 = CARTESIAN_POINT ( 'NONE',  ( -13.39048759961674229, -1.988777493506887074E-15, 0.05228750988018425472 ) ) ;
#9631 = CARTESIAN_POINT ( 'NONE',  ( 18.62499999999934630, -15.60937499999996270, 7.714727599200467800 ) ) ;
#9632 = CARTESIAN_POINT ( 'NONE',  ( -6.500262833459416356, 31.41893658545258461, -11.83852468435292238 ) ) ;
#9633 = CARTESIAN_POINT ( 'NONE',  ( 5.937628886501558512, 72.96351727730900905, -12.12413192913790994 ) ) ;
#9634 = CARTESIAN_POINT ( 'NONE',  ( 7.500000000000000888, 98.93000000000002103, 1.224646799147353059E-15 ) ) ;
#9635 = CARTESIAN_POINT ( 'NONE',  ( -13.50000000000000000, -18.06999999999999673, -3.469446951953614189E-15 ) ) ;
#9636 = CARTESIAN_POINT ( 'NONE',  ( 13.50000000000000355, 75.57999999999999829, -4.386415899144233244 ) ) ;
#9637 = CARTESIAN_POINT ( 'NONE',  ( -13.16475778499479077, 53.03611007690431478, 2.991896333637389827 ) ) ;
#9638 = CARTESIAN_POINT ( 'NONE',  ( -11.76794919243112325, 50.92999999999999972, -2.882316262207890869E-15 ) ) ;
#9639 = CARTESIAN_POINT ( 'NONE',  ( 8.343458848123578520, 64.97999999999998977, 11.48378591275254124 ) ) ;
#9640 = CARTESIAN_POINT ( 'NONE',  ( 1.449568327994486205, 50.73212129594191566, 13.42208168688401138 ) ) ;
#9641 = CARTESIAN_POINT ( 'NONE',  ( 12.79854278110677335, 69.27532975822802541, 4.295070630454624450 ) ) ;
#9642 = CARTESIAN_POINT ( 'NONE',  ( -18.62500000000064659, -9.365624999999976552, 7.714727599197335195 ) ) ;
#9643 = CARTESIAN_POINT ( 'NONE',  ( 13.30596133608670684, 36.34985342903621586, 2.280658287200722611 ) ) ;
#9644 = CARTESIAN_POINT ( 'NONE',  ( 13.16986379960055409, -25.98124999999995310, -13.16986379959834430 ) ) ;
#9645 = CARTESIAN_POINT ( 'NONE',  ( -13.01763028107069786, 74.05766348689789424, 3.576502924852020371 ) ) ;
#9646 = CARTESIAN_POINT ( 'NONE',  ( -9.698786012810412416, 76.56353993267508429, -9.394740705748864329 ) ) ;
#9647 = CARTESIAN_POINT ( 'NONE',  ( -1.645451467107404531, 7.815250021811911196, -18.85000554241877779 ) ) ;
#9648 = CARTESIAN_POINT ( 'NONE',  ( -3.737279461696752201E-15, 73.17999999999999261, -13.50000000000000000 ) ) ;
#9649 = CARTESIAN_POINT ( 'NONE',  ( 17.32050807568879236, 0.000000000000000000, -9.999999999999960920 ) ) ;
#9650 = CARTESIAN_POINT ( 'NONE',  ( 3.636496289402157078, 6.030000000000007354, -11.19198476289190936 ) ) ;
#9651 = CARTESIAN_POINT ( 'NONE',  ( -11.76794919243112325, 44.77999999999999403, -3.823638476888998827 ) ) ;
#9652 = CARTESIAN_POINT ( 'NONE',  ( 9.235079662642815990, -17.96812680894470660, 10.25657514373247814 ) ) ;
#9653 = CARTESIAN_POINT ( 'NONE',  ( -10.26398047125928059, 40.59323998322559390, -8.769304803125226755 ) ) ;
#9654 = CARTESIAN_POINT ( 'NONE',  ( -0.5908154233732432203, 34.20124354298254588, -13.50000000000000000 ) ) ;
#9655 = CARTESIAN_POINT ( 'NONE',  ( 13.37172142950504039, 75.49701186157564337, -1.917096768542019269 ) ) ;
#9656 = EDGE_CURVE ( 'NONE', #2472, #16171, #3322, .T. ) ;
#9657 = CARTESIAN_POINT ( 'NONE',  ( 4.460904823772671612, -6.117673133592659619E-13, -12.67084129013523430 ) ) ;
#9658 = LINE ( 'NONE', #13857, #10753 ) ;
#9659 = CARTESIAN_POINT ( 'NONE',  ( -11.34595542185857830, 41.20413535737528576, 7.316697782643927894 ) ) ;
#9660 = CARTESIAN_POINT ( 'NONE',  ( 0.2967297785716159764, 52.16933069184229055, -13.50000000000000355 ) ) ;
#9661 = CARTESIAN_POINT ( 'NONE',  ( 6.246728678326504358, 44.90877324909803292, 11.96783861637221946 ) ) ;
#9662 = DIRECTION ( 'NONE',  ( 0.000000000000000000, 0.000000000000000000, -1.000000000000000000 ) ) ;
#9663 = FACE_OUTER_BOUND ( 'NONE', #15671, .T. ) ;
#9664 = CARTESIAN_POINT ( 'NONE',  ( -8.291044507619272909E-14, 57.17999999999999972, -13.50000000000000000 ) ) ;
#9665 = CARTESIAN_POINT ( 'NONE',  ( -8.170351414437741155, 49.48998335967211659, -10.77201803496731181 ) ) ;
#9666 = VECTOR ( 'NONE', #9766, 1000.000000000000000 ) ;
#9667 = CARTESIAN_POINT ( 'NONE',  ( 12.85582805263922523, 63.28191613100854340, 4.121090797647687154 ) ) ;
#9668 = CARTESIAN_POINT ( 'NONE',  ( 9.124530604564489167, 42.03482481052925834, 9.963362446407785455 ) ) ;
#9669 = CARTESIAN_POINT ( 'NONE',  ( 5.573104024729542694, 48.97745214738866082, -12.29793966966750318 ) ) ;
#9670 = ORIENTED_EDGE ( 'NONE', *, *, #3504, .F. ) ;
#9671 = CARTESIAN_POINT ( 'NONE',  ( -8.891200544363830713E-16, 4.546025403784440755, 12.00000000000000000 ) ) ;
#9672 = CARTESIAN_POINT ( 'NONE',  ( -17.32050807568884210, 0.000000000000000000, 7.999999999999840128 ) ) ;
#9673 = CARTESIAN_POINT ( 'NONE',  ( 13.50000000000000355, 9.580000000000008953, -4.386415899144233244 ) ) ;
#9674 = ORIENTED_EDGE ( 'NONE', *, *, #11426, .T. ) ;
#9675 = CARTESIAN_POINT ( 'NONE',  ( -11.96708799091716280, 43.69658687964136590, -6.330084694767312392 ) ) ;
#9676 = CARTESIAN_POINT ( 'NONE',  ( -7.499999999999998224, 108.6662573213694429, 2.063574628993714022 ) ) ;
#9677 = CARTESIAN_POINT ( 'NONE',  ( 13.47423762379474610, 60.45965211740971057, -0.8577208552641553130 ) ) ;
#9678 = CARTESIAN_POINT ( 'NONE',  ( 4.171729424061789260, 15.83000000000001073, 12.83926296998457239 ) ) ;
#9679 = CARTESIAN_POINT ( 'NONE',  ( 1.653273178848926472E-15, 80.93000000000000682, 13.50000000000000000 ) ) ;
#9680 = CARTESIAN_POINT ( 'NONE',  ( 13.45263629682293782, 66.39079416573831338, 1.129939417163000615 ) ) ;
#9681 = CARTESIAN_POINT ( 'NONE',  ( 2.041061911512047189, 56.75340703010081000, 13.34548534108487061 ) ) ;
#9682 = CARTESIAN_POINT ( 'NONE',  ( -11.76794919243112325, 56.92999999999999972, -2.882316262207890869E-15 ) ) ;
#9683 = CARTESIAN_POINT ( 'NONE',  ( 7.272992578804308828, 63.97999999999998977, 10.01041549318726709 ) ) ;
#9684 = AXIS2_PLACEMENT_3D ( 'NONE', #8449, #6221, #11607 ) ;
#9685 = CARTESIAN_POINT ( 'NONE',  ( -12.37777064474171240, 47.12682678988542051, 5.391107621120311499 ) ) ;
#9686 = DIRECTION ( 'NONE',  ( 0.000000000000000000, 0.000000000000000000, 1.000000000000000000 ) ) ;
#9687 = DIRECTION ( 'NONE',  ( 0.000000000000000000, 0.000000000000000000, -1.000000000000000000 ) ) ;
#9688 = CARTESIAN_POINT ( 'NONE',  ( 10.46257632922059777, 30.75595908514958055, -8.531413285560027759 ) ) ;
#9689 = CARTESIAN_POINT ( 'NONE',  ( -10.63672848954992389, 9.999999999999994671, -6.255867060675207370 ) ) ;
#9690 = CARTESIAN_POINT ( 'NONE',  ( 4.711679271993006068, -96.77812499999976126, 11.37500000000039257 ) ) ;
#9691 = CARTESIAN_POINT ( 'NONE',  ( 12.00000000000000533, 98.93000000000002103, 1.224646799147353059E-15 ) ) ;
#9692 = CARTESIAN_POINT ( 'NONE',  ( 13.35604756179318464, 33.50086920132254420, -2.024719069001440275 ) ) ;
#9693 = CARTESIAN_POINT ( 'NONE',  ( -10.92957602604999146, 9.999999999999998224, 4.954227274842499362 ) ) ;
#9694 = CARTESIAN_POINT ( 'NONE',  ( 0.01847178140511852168, 40.17933609548848750, -13.50000000169804792 ) ) ;
#9695 = CARTESIAN_POINT ( 'NONE',  ( 3.636496289402154414, 22.83000000000001606, 11.19198476289190758 ) ) ;
#9696 = VERTEX_POINT ( 'NONE', #2383 ) ;
#9697 = CARTESIAN_POINT ( 'NONE',  ( -4.171729424061791036, 43.53000000000000114, 12.83926296998457239 ) ) ;
#9698 = ORIENTED_EDGE ( 'NONE', *, *, #1666, .T. ) ;
#9699 = AXIS2_PLACEMENT_3D ( 'NONE', #8943, #14130, #1932 ) ;
#9700 = CARTESIAN_POINT ( 'NONE',  ( 7.272992578804311492, -15.12000000000000277, -10.01041549318726709 ) ) ;
#9701 = CARTESIAN_POINT ( 'NONE',  ( -13.16986379960055409, -50.95624999999989768, 13.16986379959834252 ) ) ;
#9702 = CARTESIAN_POINT ( 'NONE',  ( -13.46309576110611239, 43.89548648200645431, -0.9975764637713919747 ) ) ;
#9703 = ADVANCED_FACE ( 'NONE', ( #3555 ), #6311, .T. ) ;
#9704 = CARTESIAN_POINT ( 'NONE',  ( 2.138189944381242213, 1.103118577679735202, -13.49999999999999822 ) ) ;
#9705 = CARTESIAN_POINT ( 'NONE',  ( -8.343458848123576743, 34.47999999999998977, -11.48378591275254301 ) ) ;
#9706 = CARTESIAN_POINT ( 'NONE',  ( -13.49999999999999822, 46.07999999999999119, 4.386415899144235908 ) ) ;
#9707 = CIRCLE ( 'NONE', #2051, 8.999999999999994671 ) ;
#9708 = CARTESIAN_POINT ( 'NONE',  ( 18.62500000000000000, -9.399999999999959499, 1.560692158462880521E-12 ) ) ;
#9709 = CARTESIAN_POINT ( 'NONE',  ( -10.25381866242074658, 67.59266383462906447, -8.782231892207333246 ) ) ;
#9710 = CARTESIAN_POINT ( 'NONE',  ( 7.714727599200456254, -62.47187499999984084, -18.62499999999935341 ) ) ;
#9711 = CARTESIAN_POINT ( 'NONE',  ( 13.05622502498204973, 54.30767452267900097, 3.432944569055587536 ) ) ;
#9712 = CARTESIAN_POINT ( 'NONE',  ( -6.044985788396838977, 64.40073192607152919, -12.07114179645960306 ) ) ;
#9713 = EDGE_LOOP ( 'NONE', ( #16661, #11899, #7946, #8083, #7474 ) ) ;
#9714 = CARTESIAN_POINT ( 'NONE',  ( -11.84369742284435212, 34.69003919059396424, -6.478953855484251179 ) ) ;
#9715 = ORIENTED_EDGE ( 'NONE', *, *, #12398, .F. ) ;
#9716 = CARTESIAN_POINT ( 'NONE',  ( 13.40174896357971690, 78.37331495776443546, 1.625770599117996040 ) ) ;
#9717 = CARTESIAN_POINT ( 'NONE',  ( 13.50000000000000000, 47.42999999999999972, 1.653273178848926867E-15 ) ) ;
#9718 = CARTESIAN_POINT ( 'NONE',  ( -13.49999999999999822, 36.78000000000000114, -4.386415899144240349 ) ) ;
#9719 = CARTESIAN_POINT ( 'NONE',  ( 2.393234054935799549, 73.09397480562172689, -13.29186828747294946 ) ) ;
#9720 = CARTESIAN_POINT ( 'NONE',  ( 6.595643076912385716, 59.92293436221358860, 11.77912079893219044 ) ) ;
#9721 = CARTESIAN_POINT ( 'NONE',  ( 9.235077742801747647, -19.96812692063823391, 10.25657778616701954 ) ) ;
#9722 = CARTESIAN_POINT ( 'NONE',  ( 10.92172942406178926, 63.12999999999998835, 7.935100905948387684 ) ) ;
#9723 = CARTESIAN_POINT ( 'NONE',  ( -11.20884234386199907, 52.64724540846238909, -7.524086072081253462 ) ) ;
#9724 = CARTESIAN_POINT ( 'NONE',  ( 3.636496289402154414, 42.82999999999999829, 11.19198476289190936 ) ) ;
#9725 = CARTESIAN_POINT ( 'NONE',  ( 13.50000000000000000, 59.42999999999999972, 1.653273178848926867E-15 ) ) ;
#9726 = FACE_OUTER_BOUND ( 'NONE', #11982, .T. ) ;
#9727 = CARTESIAN_POINT ( 'NONE',  ( 10.16932816747080714, 69.08810190452132360, 8.881946212672056973 ) ) ;
#9728 = CARTESIAN_POINT ( 'NONE',  ( -2.390223969659595493, 37.26593391360592022, -13.29042876175976140 ) ) ;
#9729 = CARTESIAN_POINT ( 'NONE',  ( 1.900613283894400762, 5.969143981464174686, -12.00000000000001599 ) ) ;
#9730 = CARTESIAN_POINT ( 'NONE',  ( -18.62500000000064659, -49.91562499999989910, 7.714727599197333419 ) ) ;
#9731 = CARTESIAN_POINT ( 'NONE',  ( -8.353752051756876185, 74.36112887588994624, 10.60510391640503158 ) ) ;
#9732 = CARTESIAN_POINT ( 'NONE',  ( -7.214465774454332347, 76.44870526399246558, -11.41059411142753177 ) ) ;
#9733 = CARTESIAN_POINT ( 'NONE',  ( -4.375655242806324452, 79.33737030707416693, -12.77121110675854787 ) ) ;
#9734 = CARTESIAN_POINT ( 'NONE',  ( -8.000000000000191847, 5.918584287042170544, 24.73863375370590134 ) ) ;
#9735 = CARTESIAN_POINT ( 'NONE',  ( -11.29885598845895878, 80.93000000000000682, 4.264693269851297153 ) ) ;
#9736 = CARTESIAN_POINT ( 'NONE',  ( 10.92172942406178926, 31.13000000000002032, 7.935100905948385908 ) ) ;
#9737 = CARTESIAN_POINT ( 'NONE',  ( -3.636496289402152637, -2.669999999999998597, -11.19198476289190936 ) ) ;
#9738 = CARTESIAN_POINT ( 'NONE',  ( -9.520470885617717371, 48.23000000000000398, 6.917026985038133624 ) ) ;
#9739 = CARTESIAN_POINT ( 'NONE',  ( -8.343458848123578520, 1.479999999999995097, -11.48378591275254124 ) ) ;
#9740 = ADVANCED_FACE ( 'NONE', ( #11697 ), #6147, .F. ) ;
#9741 = CARTESIAN_POINT ( 'NONE',  ( -0.8899778701273365344, 32.64814878773904638, 13.47798037021882500 ) ) ;
#9742 = CARTESIAN_POINT ( 'NONE',  ( 12.20100399948782055, 75.21792834827131458, 5.778299298237292270 ) ) ;
#9743 = CARTESIAN_POINT ( 'NONE',  ( 7.564450330115305654, -3.230386817174870386E-14, -15.36044013669110164 ) ) ;
#9744 = CARTESIAN_POINT ( 'NONE',  ( 2.272985001014427788E-15, 32.17999999999999972, -12.37355403259654985 ) ) ;
#9745 = CARTESIAN_POINT ( 'NONE',  ( -12.56035316918483069, 41.10966195528746425, 4.948503074325818929 ) ) ;
#9746 = CIRCLE ( 'NONE', #6357, 9.000000000000001776 ) ;
#9747 = CARTESIAN_POINT ( 'NONE',  ( 4.956108786688578682, 52.00122210954356916, -12.55763373905415392 ) ) ;
#9748 = CARTESIAN_POINT ( 'NONE',  ( -7.264190498165104870, 38.40920588462986984, 11.37994681411909781 ) ) ;
#9749 = DIRECTION ( 'NONE',  ( 0.000000000000000000, 0.000000000000000000, 1.000000000000000000 ) ) ;
#9750 = CARTESIAN_POINT ( 'NONE',  ( -18.06260399879729306, 6.548267719634618622, -15.28534784291422177 ) ) ;
#9751 = CARTESIAN_POINT ( 'NONE',  ( -7.121125983345519828, 49.44472971541036088, -11.47042538111829657 ) ) ;
#9752 = CARTESIAN_POINT ( 'NONE',  ( 9.577391939495372597, 63.05751216351371369, 9.514465974150908778 ) ) ;
#9753 = CARTESIAN_POINT ( 'NONE',  ( 13.33619231753804613, 42.35646018360174025, 2.097296710946952025 ) ) ;
#9754 = CARTESIAN_POINT ( 'NONE',  ( 4.704464924678342541, 38.84934771415909438, 12.65631601052290911 ) ) ;
#9755 = CARTESIAN_POINT ( 'NONE',  ( -3.636496289402156190, 22.52999999999999403, 11.19198476289190758 ) ) ;
#9756 = ORIENTED_EDGE ( 'NONE', *, *, #13864, .T. ) ;
#9757 = CARTESIAN_POINT ( 'NONE',  ( -7.272992578804307939, 77.48000000000000398, -10.01041549318727064 ) ) ;
#9758 = DIRECTION ( 'NONE',  ( 0.000000000000000000, -0.000000000000000000, -1.000000000000000000 ) ) ;
#9759 = CARTESIAN_POINT ( 'NONE',  ( 9.538709233711902776E-13, -54.11249999999986926, -11.37500000000000000 ) ) ;
#9760 = CARTESIAN_POINT ( 'NONE',  ( 4.171729424061791924, 7.030000000000008242, -12.83926296998457239 ) ) ;
#9761 = ORIENTED_EDGE ( 'NONE', *, *, #16269, .T. ) ;
#9762 = CARTESIAN_POINT ( 'NONE',  ( -11.13438765174952927, 43.64266397379046225, -7.633879821230919127 ) ) ;
#9763 = CARTESIAN_POINT ( 'NONE',  ( -7.500000000000000888, 106.0136413093990910, 8.254396200996682254 ) ) ;
#9764 = CARTESIAN_POINT ( 'NONE',  ( 9.400436423136840247, 60.81129539022329311, -9.689632365782298251 ) ) ;
#9765 = CARTESIAN_POINT ( 'NONE',  ( 13.49999999999999822, 1.279999999999994476, 4.386415899144237684 ) ) ;
#9766 = DIRECTION ( 'NONE',  ( -0.000000000000000000, -1.000000000000000000, -0.000000000000000000 ) ) ;
#9767 = CARTESIAN_POINT ( 'NONE',  ( 13.40858775979793194, 66.48465639307120512, -1.568604466400953301 ) ) ;
#9768 = CARTESIAN_POINT ( 'NONE',  ( -17.42428528562830792, 5.918584287042170544, -19.29752010712871169 ) ) ;
#9769 = CARTESIAN_POINT ( 'NONE',  ( -3.636496289402153081, 62.32999999999999829, -11.19198476289190936 ) ) ;
#9770 = CARTESIAN_POINT ( 'NONE',  ( 8.343458848123583849, 35.87999999999999545, -11.48378591275253768 ) ) ;
#9771 = CARTESIAN_POINT ( 'NONE',  ( -3.636496289402155746, 63.53000000000000114, 11.19198476289190936 ) ) ;
#9772 = CARTESIAN_POINT ( 'NONE',  ( -13.17996130359396645, 46.82475302137621753, -2.970985941612378500 ) ) ;
#9773 = CARTESIAN_POINT ( 'NONE',  ( 13.10097267581912206, 45.54584849643477895, -3.258082403950691042 ) ) ;
#9774 = CARTESIAN_POINT ( 'NONE',  ( 2.445080149700053643E-15, 48.17999999999999972, -13.50000000000000000 ) ) ;
#9775 = CARTESIAN_POINT ( 'NONE',  ( 1.157795017994313280, 7.956106560002609740, 18.35996578475045382 ) ) ;
#9776 = CARTESIAN_POINT ( 'NONE',  ( 11.40617213196905411, 30.70028543943833910, -7.221826826951074807 ) ) ;
#9777 = CARTESIAN_POINT ( 'NONE',  ( -9.410437633937705826, 56.31096153803149917, 9.682104401986398656 ) ) ;
#9778 = CARTESIAN_POINT ( 'NONE',  ( 4.711679271993006068, -80.12812499999981242, 11.37500000000039257 ) ) ;
#9779 = DIRECTION ( 'NONE',  ( 0.000000000000000000, 1.000000000000000000, 0.000000000000000000 ) ) ;
#9780 = CARTESIAN_POINT ( 'NONE',  ( 9.114660220015876391, 33.03466814584144373, 9.958601439926033194 ) ) ;
#9781 = CARTESIAN_POINT ( 'NONE',  ( -10.76106711467583210, 10.00000000000000000, 5.407306280985056723 ) ) ;
#9782 = CARTESIAN_POINT ( 'NONE',  ( 4.392283583417332160, 40.02202581670101011, -12.76555334419149013 ) ) ;
#9783 = CARTESIAN_POINT ( 'NONE',  ( 3.636496289402157078, 24.02999999999999403, -11.19198476289190936 ) ) ;
#9784 = ORIENTED_EDGE ( 'NONE', *, *, #16834, .T. ) ;
#9785 = CARTESIAN_POINT ( 'NONE',  ( -6.523130144822721910, 62.44009285821610433, 11.82982051691417702 ) ) ;
#9786 = VECTOR ( 'NONE', #8300, 1000.000000000000000 ) ;
#9787 = ORIENTED_EDGE ( 'NONE', *, *, #13167, .T. ) ;
#9788 = CARTESIAN_POINT ( 'NONE',  ( 18.62499999999935341, -72.80937499999984652, 7.714727599200469577 ) ) ;
#9789 = CARTESIAN_POINT ( 'NONE',  ( -13.48346897527509114, 43.95311960857426214, 0.6707733342585510128 ) ) ;
#9790 = PLANE ( 'NONE',  #13832 ) ;
#9791 = CARTESIAN_POINT ( 'NONE',  ( 10.92172942406178926, 30.12999999999999545, 7.935100905948387684 ) ) ;
#9792 = CARTESIAN_POINT ( 'NONE',  ( 8.343458848123583849, 47.88000000000000256, -11.48378591275253768 ) ) ;
#9793 = CIRCLE ( 'NONE', #12030, 26.00000000000000355 ) ;
#9794 = CARTESIAN_POINT ( 'NONE',  ( -2.552045539003058749, 46.27175948752068280, -13.25665630414003893 ) ) ;
#9795 = EDGE_CURVE ( 'NONE', #4872, #13385, #12385, .T. ) ;
#9796 = CARTESIAN_POINT ( 'NONE',  ( -9.409590922929337964, 67.54892891243062536, -9.687992896030786838 ) ) ;
#9797 = CARTESIAN_POINT ( 'NONE',  ( 18.62499999999935341, -41.65937499999989058, 7.714727599200469577 ) ) ;
#9798 = CARTESIAN_POINT ( 'NONE',  ( 0.6922064125909698218, 53.70486120015097953, 13.50000000000462919 ) ) ;
#9799 = CARTESIAN_POINT ( 'NONE',  ( -10.42167427526279688, 64.60167514499391928, -8.581475041684891281 ) ) ;
#9800 = VERTEX_POINT ( 'NONE', #7529 ) ;
#9801 = CARTESIAN_POINT ( 'NONE',  ( 15.67642540545348773, 8.062211465790062093, -8.847408738254129545 ) ) ;
#9802 = CARTESIAN_POINT ( 'NONE',  ( -11.72378450257766147, 35.17872340265273579, 6.696941732122135171 ) ) ;
#9803 = CARTESIAN_POINT ( 'NONE',  ( 8.043339635997654113, -52.03124999999987921, -8.043339635996304082 ) ) ;
#9804 = ORIENTED_EDGE ( 'NONE', *, *, #10715, .T. ) ;
#9805 = CARTESIAN_POINT ( 'NONE',  ( 13.15122240745925808, 78.31917349788055560, 3.127322199626254129 ) ) ;
#9806 = DIRECTION ( 'NONE',  ( 0.000000000000000000, -1.000000000000000000, 0.000000000000000000 ) ) ;
#9807 = CIRCLE ( 'NONE', #6419, 12.00000000000000178 ) ;
#9808 = DIRECTION ( 'NONE',  ( 0.000000000000000000, -1.000000000000000000, 0.000000000000000000 ) ) ;
#9809 = CARTESIAN_POINT ( 'NONE',  ( 9.843127303906451075, 72.78901079599570778, -9.241637740177777616 ) ) ;
#9810 = CARTESIAN_POINT ( 'NONE',  ( 4.939422578511702966, 79.00184200604905982, -12.56392261057602688 ) ) ;
#9811 = CARTESIAN_POINT ( 'NONE',  ( 2.621994543952811015E-15, -12.82000000000000206, -14.19474002721660355 ) ) ;
#9812 = CARTESIAN_POINT ( 'NONE',  ( -8.343458848123582072, 59.37999999999999545, 11.48378591275254124 ) ) ;
#9813 = CARTESIAN_POINT ( 'NONE',  ( -13.46416202051893407, 52.96403103733616291, 0.9835209988710441609 ) ) ;
#9814 = CARTESIAN_POINT ( 'NONE',  ( -7.272992578804307939, 38.47999999999999687, -10.01041549318726886 ) ) ;
#9815 = CARTESIAN_POINT ( 'NONE',  ( 0.000000000000000000, 0.000000000000000000, 0.000000000000000000 ) ) ;
#9816 = CARTESIAN_POINT ( 'NONE',  ( 4.171729424061791924, 57.02999999999999403, -12.83926296998457239 ) ) ;
#9817 = CARTESIAN_POINT ( 'NONE',  ( -17.32050807568884210, 0.000000000000000000, 7.999999999999840128 ) ) ;
#9818 = CARTESIAN_POINT ( 'NONE',  ( 3.636496289402154414, -4.169999999999999929, 11.19198476289190758 ) ) ;
#9819 = CARTESIAN_POINT ( 'NONE',  ( 9.423612524159942438, 69.04964748713040024, 9.673382742204811535 ) ) ;
#9820 = CARTESIAN_POINT ( 'NONE',  ( -7.714727599197335195, -5.203124999999987566, -18.62500000000064304 ) ) ;
#9821 = EDGE_CURVE ( 'NONE', #13302, #2326, #3450, .T. ) ;
#9822 = DIRECTION ( 'NONE',  ( 0.000000000000000000, 0.000000000000000000, -1.000000000000000000 ) ) ;
#9823 = CARTESIAN_POINT ( 'NONE',  ( 7.714727599197340524, -70.72812499999984936, 18.62500000000063949 ) ) ;
#9824 = CARTESIAN_POINT ( 'NONE',  ( -11.98704755772539698, 73.70041729349563298, -6.222936530383990750 ) ) ;
#9825 = CARTESIAN_POINT ( 'NONE',  ( -4.140906574081368419, 76.32871695187549221, -12.85379821556370850 ) ) ;
#9826 = DIRECTION ( 'NONE',  ( 0.000000000000000000, 0.000000000000000000, -1.000000000000000000 ) ) ;
#9827 = FACE_OUTER_BOUND ( 'NONE', #6862, .T. ) ;
#9828 = CARTESIAN_POINT ( 'NONE',  ( 0.7057993694277138186, 80.93000000000002103, 13.10211957505607927 ) ) ;
#9829 =( LENGTH_UNIT ( ) NAMED_UNIT ( * ) SI_UNIT ( .MILLI., .METRE. ) );
#9830 = CARTESIAN_POINT ( 'NONE',  ( -11.76794919243112325, -5.069999999999998508, -2.602085213965210642E-15 ) ) ;
#9831 = CARTESIAN_POINT ( 'NONE',  ( 11.76794919243112680, 40.57999999999999829, -3.823638476888993942 ) ) ;
#9832 = CARTESIAN_POINT ( 'NONE',  ( -10.92172942406179104, -15.76999999999999957, 7.935100905948385908 ) ) ;
#9833 = CARTESIAN_POINT ( 'NONE',  ( -1.652382928431953335, 32.62058735545888766, 13.39849679836423846 ) ) ;
#9834 = CARTESIAN_POINT ( 'NONE',  ( 13.50411512954748794, 75.43386579576426243, -0.1159153957384908701 ) ) ;
#9835 = CARTESIAN_POINT ( 'NONE',  ( 10.01414618136188217, -1.361280322109220638E-15, -6.060987932350863971 ) ) ;
#9836 = CARTESIAN_POINT ( 'NONE',  ( -3.636496289402153081, 32.32999999999999829, -11.19198476289190936 ) ) ;
#9837 = CARTESIAN_POINT ( 'NONE',  ( 10.92172942406179104, 83.73000000000000398, -7.935100905948385908 ) ) ;
#9838 = CARTESIAN_POINT ( 'NONE',  ( -1.921282587139656828, 58.24907104121455603, -13.36368293974023480 ) ) ;
#9839 = CARTESIAN_POINT ( 'NONE',  ( -2.287907212011502267, 38.59768353198680302, 13.30634456475851657 ) ) ;
#9840 = EDGE_CURVE ( 'NONE', #14181, #13443, #4431, .T. ) ;
#9841 = CARTESIAN_POINT ( 'NONE',  ( 15.58845726811984811, 0.000000000000000000, 11.00000000000007283 ) ) ;
#9842 = CARTESIAN_POINT ( 'NONE',  ( 12.50000000000000000, 98.93000000000002103, 9.000000000000000000 ) ) ;
#9843 = CARTESIAN_POINT ( 'NONE',  ( 7.124828474515464194, 62.94491023264873775, 11.46677771899573806 ) ) ;
#9844 = CARTESIAN_POINT ( 'NONE',  ( 13.09035282259576860, 42.30865731531114449, 3.417435527121966299 ) ) ;
#9845 = CARTESIAN_POINT ( 'NONE',  ( -1.003760800223034469E-07, 53.67999720368429450, 13.49999999999999822 ) ) ;
#9846 = CARTESIAN_POINT ( 'NONE',  ( 7.272992578804308828, 25.98000000000001108, 10.01041549318726709 ) ) ;
#9847 = ORIENTED_EDGE ( 'NONE', *, *, #4375, .F. ) ;
#9848 = CARTESIAN_POINT ( 'NONE',  ( 7.272992578804311492, 70.87999999999998124, -10.01041549318726886 ) ) ;
#9849 = CARTESIAN_POINT ( 'NONE',  ( -4.413477281977257860, 70.33879155025191210, -12.75886604156020177 ) ) ;
#9850 = CARTESIAN_POINT ( 'NONE',  ( 8.043339635996300530, -31.21874999999992539, 8.043339635997654113 ) ) ;
#9851 = CARTESIAN_POINT ( 'NONE',  ( 10.92172942406179104, 9.730000000000016414, -7.935100905948385908 ) ) ;
#9852 = ORIENTED_EDGE ( 'NONE', *, *, #14970, .F. ) ;
#9853 = CARTESIAN_POINT ( 'NONE',  ( -2.262111960729766835, 43.26133720115711867, -13.30912863721355244 ) ) ;
#9854 = CARTESIAN_POINT ( 'NONE',  ( -7.500000000000000888, 103.9506177843312145, -9.262340467025644841 ) ) ;
#9855 = CARTESIAN_POINT ( 'NONE',  ( 8.973903266457636363, 60.83235153706387877, -10.08882510061240190 ) ) ;
#9856 = CARTESIAN_POINT ( 'NONE',  ( 8.343458848123578520, 0.9799999999999967626, 11.48378591275254124 ) ) ;
#9857 = CARTESIAN_POINT ( 'NONE',  ( -9.708203932499371192, 7.096025403784452124, 7.053423027509678533 ) ) ;
#9858 = CARTESIAN_POINT ( 'NONE',  ( 8.728437868593859505, 66.01621931896406181, 10.29985775731656616 ) ) ;
#9859 = CARTESIAN_POINT ( 'NONE',  ( 12.06178501699019101, 57.20667319345715640, 6.066949433009045656 ) ) ;
#9860 = CARTESIAN_POINT ( 'NONE',  ( -9.520470885617717371, 60.22999999999999687, 6.917026985038133624 ) ) ;
#9861 = CARTESIAN_POINT ( 'NONE',  ( 11.76794919243112325, 70.43000000000000682, 1.441158131103945434E-15 ) ) ;
#9862 = CARTESIAN_POINT ( 'NONE',  ( -12.23227011786221929, 46.71983014421766711, -5.734458843251163174 ) ) ;
#9863 = CARTESIAN_POINT ( 'NONE',  ( 6.490407510521211343, 45.94148377923586679, -11.84091971732770610 ) ) ;
#9864 = CYLINDRICAL_SURFACE ( 'NONE', #913, 13.50000000000000000 ) ;
#9865 = CARTESIAN_POINT ( 'NONE',  ( 0.2181349388514764176, 31.17215667195195650, -13.49823986759029815 ) ) ;
#9866 = CARTESIAN_POINT ( 'NONE',  ( -2.469137722265373203, 56.59112983379784367, 13.27265035157923023 ) ) ;
#9867 = CARTESIAN_POINT ( 'NONE',  ( 8.043339635997652337, -9.331249999999993605, -8.043339635996302306 ) ) ;
#9868 = CARTESIAN_POINT ( 'NONE',  ( -1.774006486033653518, 50.61634266422996120, 13.38478036720835362 ) ) ;
#9869 = CARTESIAN_POINT ( 'NONE',  ( 13.16963777937186642, 33.32355251092941018, 3.006075874452558416 ) ) ;
#9870 = CARTESIAN_POINT ( 'NONE',  ( -9.328000102585853881, 10.00000000000000000, 7.920114137930480247 ) ) ;
#9871 = CARTESIAN_POINT ( 'NONE',  ( 0.000000000000000000, 9.000000000000000000, 0.000000000000000000 ) ) ;
#9872 = CARTESIAN_POINT ( 'NONE',  ( -7.272992578804310604, 25.38000000000000256, 10.01041549318726709 ) ) ;
#9873 = ORIENTED_EDGE ( 'NONE', *, *, #4854, .F. ) ;
#9874 = CARTESIAN_POINT ( 'NONE',  ( -13.49566855491535122, 61.91587976523243952, -0.4058878017242047997 ) ) ;
#9875 = ORIENTED_EDGE ( 'NONE', *, *, #13127, .T. ) ;
#9876 = CARTESIAN_POINT ( 'NONE',  ( 18.62500000000000000, -57.19999999999988916, 1.560692158462880521E-12 ) ) ;
#9877 = CARTESIAN_POINT ( 'NONE',  ( -12.72868174054197432, 43.76761864562406146, -4.497864774813045585 ) ) ;
#9878 = CARTESIAN_POINT ( 'NONE',  ( 0.000000000000000000, 30.93000000000001393, 0.000000000000000000 ) ) ;
#9879 = CIRCLE ( 'NONE', #5349, 6.000000000000001776 ) ;
#9880 = EDGE_CURVE ( 'NONE', #9538, #4482, #6203, .T. ) ;
#9881 = CARTESIAN_POINT ( 'NONE',  ( 4.171729424061791924, 34.03000000000000114, -12.83926296998457239 ) ) ;
#9882 = CARTESIAN_POINT ( 'NONE',  ( 13.49999999999999822, 44.27999999999999403, 4.386415899144237684 ) ) ;
#9883 = CARTESIAN_POINT ( 'NONE',  ( -4.810843242447075063, 46.35328194274109137, -12.61654248971126258 ) ) ;
#9884 = CARTESIAN_POINT ( 'NONE',  ( -2.881285544132592857, 67.28364482974733107, -13.18897454037147376 ) ) ;
#9885 = CARTESIAN_POINT ( 'NONE',  ( -7.714727599200466912, -87.44687499999976410, 18.62499999999935341 ) ) ;
#9886 = ADVANCED_BREP_SHAPE_REPRESENTATION ( '', ( #8814, #16654 ), #5681 ) ;
#9887 = CARTESIAN_POINT ( 'NONE',  ( 6.416313580321896914, 53.91553844827561193, 11.87812472618375281 ) ) ;
#9888 = AXIS2_PLACEMENT_3D ( 'NONE', #10714, #16080, #3988 ) ;
#9889 = ORIENTED_EDGE ( 'NONE', *, *, #17050, .T. ) ;
#9890 = CARTESIAN_POINT ( 'NONE',  ( -0.3906627798091588111, 64.19404671379548688, -13.49436755410429889 ) ) ;
#9891 = ORIENTED_EDGE ( 'NONE', *, *, #8401, .F. ) ;
#9892 = CARTESIAN_POINT ( 'NONE',  ( -5.364550830651251268, 34.37421519030890238, -12.38897206134628703 ) ) ;
#9893 = CARTESIAN_POINT ( 'NONE',  ( -11.37500000000000000, -58.27499999999986358, -9.545674412382054647E-13 ) ) ;
#9894 = CARTESIAN_POINT ( 'NONE',  ( 11.84730513591649448, 78.19030449563439333, 6.472368050555079577 ) ) ;
#9895 = CARTESIAN_POINT ( 'NONE',  ( -15.67642540545354990, 8.062211465790062093, 8.847408738254019411 ) ) ;
#9896 = CARTESIAN_POINT ( 'NONE',  ( -10.92172942406178926, 36.62999999999999545, -7.935100905948389460 ) ) ;
#9897 = CARTESIAN_POINT ( 'NONE',  ( 12.69466205804307002, 72.26397838323447331, 4.593265921401764373 ) ) ;
#9898 = EDGE_CURVE ( 'NONE', #6584, #6493, #9019, .T. ) ;
#9899 = CARTESIAN_POINT ( 'NONE',  ( 8.343458848123583849, -13.12000000000000099, -11.48378591275253768 ) ) ;
#9900 = CARTESIAN_POINT ( 'NONE',  ( 2.607531440858944223E-15, 58.17999999999999261, -14.19474002721660355 ) ) ;
#9901 = CARTESIAN_POINT ( 'NONE',  ( -9.271824160874588827, 52.54222379914162389, -9.814342718050605541 ) ) ;
#9902 = CARTESIAN_POINT ( 'NONE',  ( -3.636496289402153081, 41.32999999999999829, -11.19198476289190936 ) ) ;
#9903 = CARTESIAN_POINT ( 'NONE',  ( 2.607531440858944223E-15, 60.17999999999999972, -14.19474002721660355 ) ) ;
#9904 = CARTESIAN_POINT ( 'NONE',  ( 2.027675135001143936, 50.75292237657222216, 13.34755061297746082 ) ) ;
#9905 = CARTESIAN_POINT ( 'NONE',  ( -7.272992578804307939, 0.4799999999999978728, -10.01041549318726886 ) ) ;
#9906 = CARTESIAN_POINT ( 'NONE',  ( 11.64349391773129128, 69.17573428589047069, 6.832218660565160917 ) ) ;
#9907 = CARTESIAN_POINT ( 'NONE',  ( -4.129649858159847753, 37.32848282291750763, -12.85297598121887397 ) ) ;
#9908 = CARTESIAN_POINT ( 'NONE',  ( -10.92172942406179104, 73.23000000000000398, 7.935100905948387684 ) ) ;
#9909 = CARTESIAN_POINT ( 'NONE',  ( 1.561832610794586740E-12, -78.01249999999983231, -18.62500000000000000 ) ) ;
#9910 = CARTESIAN_POINT ( 'NONE',  ( -12.59327613556072833, 73.75357011053149847, -4.864702328253065033 ) ) ;
#9911 = CARTESIAN_POINT ( 'NONE',  ( -1.739642266260832848, 76.24253143227396379, -13.38915460456405349 ) ) ;
#9912 = DIRECTION ( 'NONE',  ( 0.000000000000000000, 0.000000000000000000, -1.000000000000000000 ) ) ;
#9913 = AXIS2_PLACEMENT_3D ( 'NONE', #11818, #17197, #6174 ) ;
#9914 = CARTESIAN_POINT ( 'NONE',  ( -8.343458848123582072, 3.380000000000000782, 11.48378591275253768 ) ) ;
#9915 = CARTESIAN_POINT ( 'NONE',  ( -7.409984580736203970E-16, -4.320000000000003837, 12.37355403259654985 ) ) ;
#9916 = CARTESIAN_POINT ( 'NONE',  ( 9.520470885617717371, 34.72999999999999687, -6.917026985038131848 ) ) ;
#9917 = CARTESIAN_POINT ( 'NONE',  ( 2.621994543952811015E-15, -16.82000000000000028, -14.19474002721660355 ) ) ;
#9918 = CARTESIAN_POINT ( 'NONE',  ( -10.77958242724814575, 32.23934130396135345, 8.159047414433960199 ) ) ;
#9919 = CARTESIAN_POINT ( 'NONE',  ( 6.634635836420705424, 74.92436317536002832, 11.76700430428859612 ) ) ;
#9920 = EDGE_CURVE ( 'NONE', #17255, #15482, #12460, .T. ) ;
#9921 = CARTESIAN_POINT ( 'NONE',  ( 10.83524660546097351, -5.362028352459062835E-15, -14.01674796189367100 ) ) ;
#9922 = CARTESIAN_POINT ( 'NONE',  ( 11.76794919243112325, 31.27999999999998693, 3.823638476888996607 ) ) ;
#9923 = CARTESIAN_POINT ( 'NONE',  ( 4.171729424061791924, 81.03000000000000114, -12.83926296998457239 ) ) ;
#9924 = CARTESIAN_POINT ( 'NONE',  ( 10.71722923847700315, 51.74181331124376726, -8.212034718187664950 ) ) ;
#9925 = DIRECTION ( 'NONE',  ( 0.000000000000000000, -1.000000000000000000, 0.000000000000000000 ) ) ;
#9926 = CARTESIAN_POINT ( 'NONE',  ( 1.732050807568875195, 0.000000000000000000, -19.00000000000000000 ) ) ;
#9927 = CARTESIAN_POINT ( 'NONE',  ( 1.653273178848926472E-15, 3.999999999999961808, 13.50000000000000000 ) ) ;
#9928 = DIRECTION ( 'NONE',  ( -0.000000000000000000, 1.000000000000000000, -0.000000000000000000 ) ) ;
#9929 = CARTESIAN_POINT ( 'NONE',  ( 3.564950917667821351, 62.80727969005073419, 13.05038946788975984 ) ) ;
#9930 = CARTESIAN_POINT ( 'NONE',  ( -8.891200544363830713E-16, 46.67999999999999972, 13.50000000000000000 ) ) ;
#9931 = CARTESIAN_POINT ( 'NONE',  ( 10.27029722546964763, 48.76660342709478613, -8.769633602492632463 ) ) ;
#9932 = CARTESIAN_POINT ( 'NONE',  ( 7.272992578804308828, 19.98000000000000043, 10.01041549318726709 ) ) ;
#9933 = VERTEX_POINT ( 'NONE', #1917 ) ;
#9934 = CARTESIAN_POINT ( 'NONE',  ( -7.272992578804307939, 65.47999999999998977, -10.01041549318727064 ) ) ;
#9935 = CARTESIAN_POINT ( 'NONE',  ( 18.62500000000000000, -92.64999999999974989, 1.560692158462880521E-12 ) ) ;
#9936 = CARTESIAN_POINT ( 'NONE',  ( 9.538709233711902776E-13, -37.46249999999991331, -11.37500000000000000 ) ) ;
#9937 = CARTESIAN_POINT ( 'NONE',  ( -8.549982208541774191E-16, 5.680000000000001492, 14.19474002721660355 ) ) ;
#9938 = ORIENTED_EDGE ( 'NONE', *, *, #8401, .T. ) ;
#9939 = CARTESIAN_POINT ( 'NONE',  ( -1.200094164391137586, 43.22314455631953223, -13.44841224794836343 ) ) ;
#9940 = CARTESIAN_POINT ( 'NONE',  ( 6.767892274116773521, 80.93000000001259764, -11.68099457092376348 ) ) ;
#9941 = CARTESIAN_POINT ( 'NONE',  ( -8.343458848123576743, 2.479999999999999982, -11.48378591275254301 ) ) ;
#9942 = DIRECTION ( 'NONE',  ( -0.000000000000000000, -1.000000000000000000, -0.000000000000000000 ) ) ;
#9943 = DIRECTION ( 'NONE',  ( 1.000000000000000000, 0.000000000000000000, 3.741588754404568134E-15 ) ) ;
#9944 = CARTESIAN_POINT ( 'NONE',  ( 7.591558717369741416, 65.96485550035102108, 11.16641294781561378 ) ) ;
#9945 = CARTESIAN_POINT ( 'NONE',  ( 11.76850315208348796, 57.18434826636972446, 6.628006218653733406 ) ) ;
#9946 = CARTESIAN_POINT ( 'NONE',  ( -9.520470885617715595, 56.63000000000000256, -6.917026985038136289 ) ) ;
#9947 = CARTESIAN_POINT ( 'NONE',  ( 7.272992578804311492, 67.87999999999999545, -10.01041549318726709 ) ) ;
#9948 = CARTESIAN_POINT ( 'NONE',  ( -13.30473318507969438, 46.84958455783641540, -2.288076029142007695 ) ) ;
#9949 = CARTESIAN_POINT ( 'NONE',  ( 9.548081290227049323, 45.80397646740897244, -9.544521494561665875 ) ) ;
#9950 = LINE ( 'NONE', #4886, #6850 ) ;
#9951 = CARTESIAN_POINT ( 'NONE',  ( 1.297534681090666941, 7.924607901204606009, 18.46823281779985848 ) ) ;
#9952 = CARTESIAN_POINT ( 'NONE',  ( 7.160989524558149633, 30.91366021522728147, -11.45163515356361650 ) ) ;
#9953 = CARTESIAN_POINT ( 'NONE',  ( -11.07142767505757419, 56.22114726484812763, 7.724863410134291897 ) ) ;
#9954 = DIRECTION ( 'NONE',  ( 0.000000000000000000, 0.000000000000000000, 1.000000000000000000 ) ) ;
#9955 = CARTESIAN_POINT ( 'NONE',  ( 8.929833117994236957, 33.02572749855196577, 10.12741600962044153 ) ) ;
#9956 = CARTESIAN_POINT ( 'NONE',  ( -3.145802693531244643, 10.00000000000000533, 12.35297229877298086 ) ) ;
#9957 = CARTESIAN_POINT ( 'NONE',  ( 8.544410748096753494, 39.85237042391017326, -10.45276505990612215 ) ) ;
#9958 = ORIENTED_EDGE ( 'NONE', *, *, #3175, .F. ) ;
#9959 = CARTESIAN_POINT ( 'NONE',  ( -11.07323960031809484, 62.22103888625681378, 7.722276753161360752 ) ) ;
#9960 = EDGE_LOOP ( 'NONE', ( #2912, #6404 ) ) ;
#9961 = CARTESIAN_POINT ( 'NONE',  ( -7.272992578804310604, -13.62000000000000632, 10.01041549318726709 ) ) ;
#9962 = CARTESIAN_POINT ( 'NONE',  ( -18.62499999999935341, -31.18437499999994600, -7.714727599200458030 ) ) ;
#9963 = CARTESIAN_POINT ( 'NONE',  ( 10.67437249253150355, 48.11583226118976597, 8.265000984528860783 ) ) ;
#9964 = AXIS2_PLACEMENT_3D ( 'NONE', #10452, #12916, #3537 ) ;
#9965 = CARTESIAN_POINT ( 'NONE',  ( 0.000000000000000000, 80.93000000000000682, -13.50000000000000000 ) ) ;
#9966 = CARTESIAN_POINT ( 'NONE',  ( -8.691771469529815392E-16, 32.67999999999999261, 14.19474002721660355 ) ) ;
#9967 = CARTESIAN_POINT ( 'NONE',  ( -13.49999999999999822, 39.77999999999998693, -4.386415899144240349 ) ) ;
#9968 = CARTESIAN_POINT ( 'NONE',  ( -5.667667140658918967, 46.38572788627769938, -12.25425454852370422 ) ) ;
#9969 = CARTESIAN_POINT ( 'NONE',  ( -11.07701847939493689, 67.63915826389134622, -7.717748835311455835 ) ) ;
#9970 = CARTESIAN_POINT ( 'NONE',  ( 1.561832610794586740E-12, -46.86249999999987637, -18.62500000000000000 ) ) ;
#9971 =( BOUNDED_CURVE ( )  B_SPLINE_CURVE ( 2, ( #9429, #5532, #11005, #13808, #8276, #14778, #302, #16189, #2668, #13722, #5712, #8100, #13465 ),
 .UNSPECIFIED., .F., .F. ) 
 B_SPLINE_CURVE_WITH_KNOTS ( ( 3, 2, 2, 2, 2, 2, 3 ),
 ( 0.5972222222222222099, 0.5999999999999999778, 0.6055555555555555136, 0.6111111111111111605, 0.6166666666666666963, 0.6222222222222222321, 0.6250000000000000000 ),
 .UNSPECIFIED. ) 
 CURVE ( )  GEOMETRIC_REPRESENTATION_ITEM ( )  RATIONAL_B_SPLINE_CURVE ( ( 0.9755282581475768211, 0.9755282581475768211, 1.000000000000000000, 0.9510565162951535312, 1.000000000000000000, 0.9510565162951535312, 1.000000000000000000, 0.9510565162951535312, 1.000000000000000000, 0.9510565162951535312, 1.000000000000000000, 0.9755282581475768211, 0.9755282581475768211 ) ) 
 REPRESENTATION_ITEM ( '' )  );
#9972 = CARTESIAN_POINT ( 'NONE',  ( 6.589847531046439499, 53.92267567950827356, 11.78235791658461018 ) ) ;
#9973 = EDGE_CURVE ( 'NONE', #1729, #14883, #5841, .T. ) ;
#9974 = ORIENTED_EDGE ( 'NONE', *, *, #12859, .T. ) ;
#9975 = CARTESIAN_POINT ( 'NONE',  ( -6.821948058657442360, 64.43206303487275477, -11.66090654277045147 ) ) ;
#9976 = ORIENTED_EDGE ( 'NONE', *, *, #3408, .T. ) ;
#9977 = DIRECTION ( 'NONE',  ( -0.000000000000000000, -1.000000000000000000, -0.000000000000000000 ) ) ;
#9978 = CARTESIAN_POINT ( 'NONE',  ( -9.272717293934437777, 34.54199207297656216, -9.829925356530168301 ) ) ;
#9979 = CARTESIAN_POINT ( 'NONE',  ( -11.37499999999960387, -73.88437499999982094, -4.711679271994910323 ) ) ;
#9980 = LINE ( 'NONE', #14269, #416 ) ;
#9981 = CARTESIAN_POINT ( 'NONE',  ( -16.64104048077470210, 7.924936010579560097, 8.111079018422834963 ) ) ;
#9982 = FACE_OUTER_BOUND ( 'NONE', #12069, .T. ) ;
#9983 = CARTESIAN_POINT ( 'NONE',  ( -13.50000000000000000, 36.92999999999999972, -3.306546357697853733E-15 ) ) ;
#9984 = CARTESIAN_POINT ( 'NONE',  ( 12.82313912373315468, 72.27809372985406355, 4.222047920560166645 ) ) ;
#9985 = CARTESIAN_POINT ( 'NONE',  ( 3.636496289402157078, 30.03000000000000114, -11.19198476289190936 ) ) ;
#9986 = CARTESIAN_POINT ( 'NONE',  ( 2.607531440858944223E-15, 64.18000000000000682, -14.19474002721660355 ) ) ;
#9987 = CARTESIAN_POINT ( 'NONE',  ( -7.191928855478868066, 52.44777283673647617, -11.43442037222222396 ) ) ;
#9988 = CIRCLE ( 'NONE', #6874, 1.999999999999997335 ) ;
#9989 = CARTESIAN_POINT ( 'NONE',  ( -3.636496289402153081, 38.32999999999999829, -11.19198476289190936 ) ) ;
#9990 = CARTESIAN_POINT ( 'NONE',  ( -11.76794919243112325, -16.92000000000000526, 3.823638476888994386 ) ) ;
#9991 = CARTESIAN_POINT ( 'NONE',  ( 10.92172942406179104, 53.72999999999999687, -7.935100905948385908 ) ) ;
#9992 = CARTESIAN_POINT ( 'NONE',  ( 1.882898711538667502, 50.74770853775734736, 13.36896204807974975 ) ) ;
#9993 = CARTESIAN_POINT ( 'NONE',  ( -11.76794919243112325, -5.220000000000004192, -3.823638476888998827 ) ) ;
#9994 = CARTESIAN_POINT ( 'NONE',  ( 3.556863673587017161, 68.80789220201475587, 13.02300793823324554 ) ) ;
#9995 = CARTESIAN_POINT ( 'NONE',  ( 1.561832610794586538E-12, -4.162499999999989875, -18.62500000000000000 ) ) ;
#9996 = CARTESIAN_POINT ( 'NONE',  ( 18.62499999999935341, -106.1093749999997868, 7.714727599200469577 ) ) ;
#9997 = CARTESIAN_POINT ( 'NONE',  ( -13.34960103463238568, 73.85960930300998939, -2.009550310400444850 ) ) ;
#9998 = CARTESIAN_POINT ( 'NONE',  ( -2.380313741584730192, 76.26558729244737833, -13.28849608079124600 ) ) ;
#9999 = CARTESIAN_POINT ( 'NONE',  ( 0.000000000000000000, -22.00000000000000000, 0.000000000000000000 ) ) ;
#10000 = CARTESIAN_POINT ( 'NONE',  ( -8.891200544363830713E-16, 64.67999999999999261, 13.50000000000000000 ) ) ;
#10001 = CARTESIAN_POINT ( 'NONE',  ( 0.000000000000000000, 0.000000000000000000, 0.000000000000000000 ) ) ;
#10002 = CARTESIAN_POINT ( 'NONE',  ( 11.76794919243112325, -3.720000000000000195, 3.823638476888996163 ) ) ;
#10003 = CARTESIAN_POINT ( 'NONE',  ( 3.636496289402157078, 38.03000000000000114, -11.19198476289190936 ) ) ;
#10004 = UNCERTAINTY_MEASURE_WITH_UNIT (LENGTH_MEASURE( 1.000000000000000082E-05 ), #15008, 'distance_accuracy_value', 'NONE');
#10005 = CARTESIAN_POINT ( 'NONE',  ( -6.299567892059761753, -18.60957387106638450, 19.22554806868047805 ) ) ;
#10006 = CARTESIAN_POINT ( 'NONE',  ( -9.397593110749021150, 32.31148091487975194, 9.692029560030380964 ) ) ;
#10007 = CARTESIAN_POINT ( 'NONE',  ( 7.473239715704042219, 74.95973476016609993, 11.24660702021163061 ) ) ;
#10008 = CARTESIAN_POINT ( 'NONE',  ( 11.37500000000000000, -9.629649721936179265E-32, 9.531744055041752924E-13 ) ) ;
#10009 = CARTESIAN_POINT ( 'NONE',  ( -8.691771469529815392E-16, 79.67999999999997840, 14.19474002721660355 ) ) ;
#10010 = LINE ( 'NONE', #8333, #12378 ) ;
#10011 = DIRECTION ( 'NONE',  ( 0.000000000000000000, -1.000000000000000000, 0.000000000000000000 ) ) ;
#10012 = CARTESIAN_POINT ( 'NONE',  ( 8.199628251150381075, 36.86814087517738159, -10.72470370097659398 ) ) ;
#10013 = ADVANCED_FACE ( 'NONE', ( #7162 ), #7246, .T. ) ;
#10014 = CARTESIAN_POINT ( 'NONE',  ( -4.171729424061787483, 69.32999999999999829, -12.83926296998457417 ) ) ;
#10015 = DIRECTION ( 'NONE',  ( 0.000000000000000000, 0.000000000000000000, 1.000000000000000000 ) ) ;
#10016 = CARTESIAN_POINT ( 'NONE',  ( 2.670759995370414419, 62.77599826986443787, 13.23319200665662265 ) ) ;
#10017 = CARTESIAN_POINT ( 'NONE',  ( 5.457920679380044326, 41.87780726792447439, 12.34751621698460156 ) ) ;
#10018 = CARTESIAN_POINT ( 'NONE',  ( 13.08319187888859325, 48.54904885850037743, -3.341727267560921977 ) ) ;
#10019 = CARTESIAN_POINT ( 'NONE',  ( -7.409984580736203970E-16, 19.68000000000001393, 12.37355403259654985 ) ) ;
#10020 = ORIENTED_EDGE ( 'NONE', *, *, #1385, .T. ) ;
#10021 = CARTESIAN_POINT ( 'NONE',  ( 3.636496289402157078, 71.03000000000000114, -11.19198476289190936 ) ) ;
#10022 = CARTESIAN_POINT ( 'NONE',  ( 11.37500000000039613, -27.09062499999992113, -4.711679271993004292 ) ) ;
#10023 = CARTESIAN_POINT ( 'NONE',  ( 9.538709233711902776E-13, -87.41249999999979536, -11.37500000000000000 ) ) ;
#10024 = CARTESIAN_POINT ( 'NONE',  ( 13.50000000000000000, 3.430000000000016591, 1.734723475976807094E-15 ) ) ;
#10025 = LINE ( 'NONE', #11250, #2653 ) ;
#10026 = CARTESIAN_POINT ( 'NONE',  ( 0.8512332319012331228, 76.14939279630267777, -13.47313715764315312 ) ) ;
#10027 = CARTESIAN_POINT ( 'NONE',  ( 13.50000000000000355, -1.420000000000000373, -4.386415899144233244 ) ) ;
#10028 = CARTESIAN_POINT ( 'NONE',  ( -13.16986379960055231, -27.05624999999993463, 13.16986379959834252 ) ) ;
#10029 = AXIS2_PLACEMENT_3D ( 'NONE', #9634, #10768, #16131 ) ;
#10030 = CARTESIAN_POINT ( 'NONE',  ( 12.89805136966890053, 66.28698917251486478, 3.986448665878211894 ) ) ;
#10031 = CARTESIAN_POINT ( 'NONE',  ( 2.607531440858944223E-15, 79.17999999999997840, -14.19474002721660355 ) ) ;
#10032 = CARTESIAN_POINT ( 'NONE',  ( 2.272985001014427788E-15, 53.17999999999999972, -12.37355403259654985 ) ) ;
#10033 = CARTESIAN_POINT ( 'NONE',  ( 13.50000000000000355, 32.57999999999999119, -4.386415899144233244 ) ) ;
#10034 = CARTESIAN_POINT ( 'NONE',  ( 3.636496289402154414, 57.82999999999999829, 11.19198476289190936 ) ) ;
#10035 = CARTESIAN_POINT ( 'NONE',  ( -11.15932890281731815, 46.64414198115739651, -7.597908150188835030 ) ) ;
#10036 = CARTESIAN_POINT ( 'NONE',  ( 10.56300723442443434, 45.75040630519399798, -8.406898149203419379 ) ) ;
#10037 = CARTESIAN_POINT ( 'NONE',  ( 5.256946664302129868, 69.98959847328292483, -12.43489626292463690 ) ) ;
#10038 = CARTESIAN_POINT ( 'NONE',  ( 11.61781901815139406, 30.68619861389073122, -6.878981689902905039 ) ) ;
#10039 = CARTESIAN_POINT ( 'NONE',  ( -12.29415991002589337, 55.72589537594633669, -5.581494872401155050 ) ) ;
#10040 = EDGE_CURVE ( 'NONE', #11330, #14612, #17194, .T. ) ;
#10041 = FACE_OUTER_BOUND ( 'NONE', #3475, .T. ) ;
#10042 = CARTESIAN_POINT ( 'NONE',  ( 4.183988668469575956, 32.83044184657291709, 12.83530497071244625 ) ) ;
#10043 = CARTESIAN_POINT ( 'NONE',  ( 2.914149619088002741, 43.07521792508150327, -13.18172077187604074 ) ) ;
#10044 = CARTESIAN_POINT ( 'NONE',  ( 11.95191583910591326, 39.66185494719976390, -6.277078602806502872 ) ) ;
#10045 = ORIENTED_EDGE ( 'NONE', *, *, #11403, .T. ) ;
#10046 = CARTESIAN_POINT ( 'NONE',  ( -11.12255880151802145, 62.21805859032765795, 7.651163739834599298 ) ) ;
#10047 = ORIENTED_EDGE ( 'NONE', *, *, #3945, .T. ) ;
#10048 = CARTESIAN_POINT ( 'NONE',  ( 9.520470885617715595, -18.86999999999999744, 6.917026985038135400 ) ) ;
#10049 = CARTESIAN_POINT ( 'NONE',  ( -18.62500000000064659, -99.86562499999978115, 7.714727599197333419 ) ) ;
#10050 = CARTESIAN_POINT ( 'NONE',  ( 11.67577013789725271, 48.17798356650521185, 6.776969691758181646 ) ) ;
#10051 = DIRECTION ( 'NONE',  ( 8.659560562354952580E-17, 0.7071067811865460184, -0.7071067811865490160 ) ) ;
#10052 = CARTESIAN_POINT ( 'NONE',  ( 2.607531440858944223E-15, 37.17999999999999972, -14.19474002721660355 ) ) ;
#10053 = CARTESIAN_POINT ( 'NONE',  ( 13.50000000000000000, 38.42999999999999972, 1.653273178848926867E-15 ) ) ;
#10054 = CARTESIAN_POINT ( 'NONE',  ( 8.378362625313673817, -1.749711886770878784E-15, 10.58551083881864407 ) ) ;
#10055 = CARTESIAN_POINT ( 'NONE',  ( -2.429978037473502273, 46.26737343488397869, -13.27956662434927537 ) ) ;
#10056 = DIRECTION ( 'NONE',  ( 0.000000000000000000, 0.000000000000000000, -1.000000000000000000 ) ) ;
#10057 = CARTESIAN_POINT ( 'NONE',  ( 4.711679271994911211, -12.52187499999995524, -11.37499999999960743 ) ) ;
#10058 = VECTOR ( 'NONE', #13936, 1000.000000000000000 ) ;
#10059 = EDGE_CURVE ( 'NONE', #7647, #11272, #2501, .T. ) ;
#10060 = CARTESIAN_POINT ( 'NONE',  ( 10.69437805966615151, 54.11696481419528482, 8.238956478643013170 ) ) ;
#10061 = ORIENTED_EDGE ( 'NONE', *, *, #5823, .T. ) ;
#10062 = CARTESIAN_POINT ( 'NONE',  ( -5.956643919577332191, 64.39723371421132470, -12.11484513224996817 ) ) ;
#10063 = ORIENTED_EDGE ( 'NONE', *, *, #7336, .T. ) ;
#10064 = CARTESIAN_POINT ( 'NONE',  ( 5.469506025976357044, 66.98182939450360607, -12.34254299208515704 ) ) ;
#10065 = CARTESIAN_POINT ( 'NONE',  ( -8.704249455524918133, 34.51507978907589091, -10.32029972064792567 ) ) ;
#10066 = CARTESIAN_POINT ( 'NONE',  ( -11.37499999999960210, -14.53437499999998295, -4.711679271994911211 ) ) ;
#10067 = CARTESIAN_POINT ( 'NONE',  ( 2.446671206298333789, 77.76795475725374729, 13.27830564658316170 ) ) ;
#10068 = CARTESIAN_POINT ( 'NONE',  ( 4.171729424061789260, 46.82999999999999829, 12.83926296998457417 ) ) ;
#10069 = CARTESIAN_POINT ( 'NONE',  ( -8.291044507619272909E-14, 7.180000000000005045, -13.50000000000000000 ) ) ;
#10070 = CARTESIAN_POINT ( 'NONE',  ( 7.500000000000003553, -25.08439332921293996, -8.253836299850741298 ) ) ;
#10071 = CARTESIAN_POINT ( 'NONE',  ( 10.67780330962509616, 72.11603026634840319, 8.260421498307383814 ) ) ;
#10072 = CARTESIAN_POINT ( 'NONE',  ( -11.76794919243112325, 28.08000000000000540, 3.823638476888994386 ) ) ;
#10073 = CARTESIAN_POINT ( 'NONE',  ( 10.92172942406179104, 66.73000000000000398, -7.935100905948385908 ) ) ;
#10074 = CARTESIAN_POINT ( 'NONE',  ( -9.971012074513973644, 52.57671928602155731, -9.134421619915956470 ) ) ;
#10075 = CARTESIAN_POINT ( 'NONE',  ( 9.520470885617717371, 34.72999999999999687, -6.917026985038131848 ) ) ;
#10076 = CARTESIAN_POINT ( 'NONE',  ( -10.92172942406179104, 55.23000000000000398, 7.935100905948387684 ) ) ;
#10077 = DIRECTION ( 'NONE',  ( -0.000000000000000000, -1.000000000000000000, -0.000000000000000000 ) ) ;
#10078 = CARTESIAN_POINT ( 'NONE',  ( 7.272992578804308828, -1.020000000000005347, 10.01041549318726709 ) ) ;
#10079 = CARTESIAN_POINT ( 'NONE',  ( -1.193958653162214389, 68.63708644905558742, 13.44710585900690525 ) ) ;
#10080 = CARTESIAN_POINT ( 'NONE',  ( -1.564113515457998572E-12, -29.13749999999993179, 18.62500000000000000 ) ) ;
#10081 = CARTESIAN_POINT ( 'NONE',  ( 18.06260399879740675, 6.548267719634615958, 15.28534784291409387 ) ) ;
#10082 = CARTESIAN_POINT ( 'NONE',  ( 7.714727599200456254, -76.97187499999985505, -18.62499999999935341 ) ) ;
#10083 = CARTESIAN_POINT ( 'NONE',  ( -13.13316445793458698, 73.81725464365611344, -3.175556518140508100 ) ) ;
#10084 = AXIS2_PLACEMENT_3D ( 'NONE', #9691, #11094, #1439 ) ;
#10085 = DIRECTION ( 'NONE',  ( -1.772429021826857464E-16, 1.000000000000000000, 0.000000000000000000 ) ) ;
#10086 = FACE_OUTER_BOUND ( 'NONE', #8929, .T. ) ;
#10087 = CARTESIAN_POINT ( 'NONE',  ( -10.92172942406178926, 2.629999999999993676, -7.935100905948389460 ) ) ;
#10088 = CARTESIAN_POINT ( 'NONE',  ( 11.76794919243112325, 37.28000000000000114, 3.823638476888997051 ) ) ;
#10089 = DIRECTION ( 'NONE',  ( -0.000000000000000000, -1.000000000000000000, -0.000000000000000000 ) ) ;
#10090 = CARTESIAN_POINT ( 'NONE',  ( -7.287599271325371220, 32.40820039520880158, 11.36473193426337680 ) ) ;
#10091 = CARTESIAN_POINT ( 'NONE',  ( 3.229257234301759816, 74.79610684415503385, 13.10849085500428224 ) ) ;
#10092 = CARTESIAN_POINT ( 'NONE',  ( -0.3097317755527617678, 53.66886317309062093, 13.49645795284958716 ) ) ;
#10093 = AXIS2_PLACEMENT_3D ( 'NONE', #1018, #10492, #6428 ) ;
#10094 = DIRECTION ( 'NONE',  ( 0.000000000000000000, 0.000000000000000000, 1.000000000000000000 ) ) ;
#10095 = CARTESIAN_POINT ( 'NONE',  ( 9.520470885617715595, 31.12999999999999901, 6.917026985038134512 ) ) ;
#10096 = CARTESIAN_POINT ( 'NONE',  ( 11.72376580509998512, 51.67863134643251755, -6.693536803949124092 ) ) ;
#10097 = LINE ( 'NONE', #6030, #13230 ) ;
#10098 = CARTESIAN_POINT ( 'NONE',  ( 7.321629298432528188, 36.90676912180014568, -11.34569854295486202 ) ) ;
#10099 = CARTESIAN_POINT ( 'NONE',  ( -13.49999999999999822, 70.07999999999999829, 4.386415899144235020 ) ) ;
#10100 = LINE ( 'NONE', #12824, #14845 ) ;
#10101 = CARTESIAN_POINT ( 'NONE',  ( 0.6841847586525967584, 62.70460016233664646, 13.48383326463766529 ) ) ;
#10102 = CARTESIAN_POINT ( 'NONE',  ( 0.000000000000000000, 80.93000000000000682, 0.000000000000000000 ) ) ;
#10103 = CARTESIAN_POINT ( 'NONE',  ( 13.23629157939490675, 48.52372149559199954, -2.655358675363076237 ) ) ;
#10104 = CARTESIAN_POINT ( 'NONE',  ( -11.76794919243112325, 18.93000000000000327, -2.602085213965210642E-15 ) ) ;
#10105 = VERTEX_POINT ( 'NONE', #14997 ) ;
#10106 = CARTESIAN_POINT ( 'NONE',  ( 11.76794919243112325, 64.43000000000000682, 1.441158131103945434E-15 ) ) ;
#10107 = CARTESIAN_POINT ( 'NONE',  ( -8.043339635997654113, -36.45624999999989768, 8.043339635996304082 ) ) ;
#10108 = CARTESIAN_POINT ( 'NONE',  ( 8.043339635997654113, -68.68124999999983515, -8.043339635996304082 ) ) ;
#10109 = CARTESIAN_POINT ( 'NONE',  ( 3.636496289402157078, 33.03000000000000114, -11.19198476289190936 ) ) ;
#10110 = CARTESIAN_POINT ( 'NONE',  ( -8.000000000000191847, 5.918584287042170544, 24.73863375370590134 ) ) ;
#10111 = CARTESIAN_POINT ( 'NONE',  ( -7.714727599200466912, -61.39687499999985221, 18.62499999999934985 ) ) ;
#10112 = CARTESIAN_POINT ( 'NONE',  ( 5.912581530857422329, 65.89548293010727775, 12.13714109508869221 ) ) ;
#10113 = CARTESIAN_POINT ( 'NONE',  ( 8.343458848123583849, 78.88000000000000966, -11.48378591275253768 ) ) ;
#10114 = EDGE_CURVE ( 'NONE', #16561, #5051, #3080, .T. ) ;
#10115 = CARTESIAN_POINT ( 'NONE',  ( 9.520470885617715595, 52.12999999999999545, 6.917026985038134512 ) ) ;
#10116 = CARTESIAN_POINT ( 'NONE',  ( -9.701085253511761763, 46.56373681230299866, -9.388382066297427997 ) ) ;
#10117 = CARTESIAN_POINT ( 'NONE',  ( 13.08346865036885731, 45.54843980811354953, -3.328194816465799288 ) ) ;
#10118 = DIRECTION ( 'NONE',  ( -0.8660254037844383745, 0.000000000000000000, -0.5000000000000006661 ) ) ;
#10119 = CARTESIAN_POINT ( 'NONE',  ( 2.207926304393408011E-15, 8.062177826491096155, 17.99999999999999645 ) ) ;
#10120 = CARTESIAN_POINT ( 'NONE',  ( 12.02455442308676759, 30.65625020179192717, -6.136782126200483134 ) ) ;
#10121 = CARTESIAN_POINT ( 'NONE',  ( -12.88168228059477727, 56.07516734758430488, 4.043721559897264228 ) ) ;
#10122 = CARTESIAN_POINT ( 'NONE',  ( -2.177972351186602040, 50.60165681262385107, 13.32324697659018575 ) ) ;
#10123 = CARTESIAN_POINT ( 'NONE',  ( 9.340143388868789032, 33.04566569248647312, 9.748318470567989280 ) ) ;
#10124 = CARTESIAN_POINT ( 'NONE',  ( 3.131226932223059034, 43.06742001594902547, -13.13221980506242303 ) ) ;
#10125 = CARTESIAN_POINT ( 'NONE',  ( 10.26973110394399846, 39.76645578949973014, -8.762594870586800866 ) ) ;
#10126 = ORIENTED_EDGE ( 'NONE', *, *, #10503, .F. ) ;
#10127 = CARTESIAN_POINT ( 'NONE',  ( -13.47444954086344815, 61.90133406425022145, -0.8302180661310076815 ) ) ;
#10128 = ORIENTED_EDGE ( 'NONE', *, *, #56, .T. ) ;
#10129 = ORIENTED_EDGE ( 'NONE', *, *, #9821, .T. ) ;
#10130 = CARTESIAN_POINT ( 'NONE',  ( 10.92172942406178926, 30.13000000000001677, 7.935100905948385908 ) ) ;
#10131 = CARTESIAN_POINT ( 'NONE',  ( 7.714727599197338748, -13.52812499999996732, 18.62500000000063949 ) ) ;
#10132 = CARTESIAN_POINT ( 'NONE',  ( 10.28365721251559606, 48.09423968048177045, 8.748761603325048597 ) ) ;
#10133 = CARTESIAN_POINT ( 'NONE',  ( 4.708533875543480463, 58.01043352540193609, -12.65229227841353676 ) ) ;
#10134 = CARTESIAN_POINT ( 'NONE',  ( 9.473773279193389740, 78.80763578817767723, -9.618192038280239942 ) ) ;
#10135 = CARTESIAN_POINT ( 'NONE',  ( 11.76794919243112680, 82.58000000000001251, -3.823638476888993942 ) ) ;
#10136 = CARTESIAN_POINT ( 'NONE',  ( -13.49999999999999822, 40.07999999999999829, 4.386415899144235908 ) ) ;
#10137 = EDGE_CURVE ( 'NONE', #5802, #6127, #12162, .T. ) ;
#10138 = AXIS2_PLACEMENT_3D ( 'NONE', #327, #7144, #13919 ) ;
#10139 = CARTESIAN_POINT ( 'NONE',  ( -9.620323683735932718, 46.55968297308034209, -9.470975885656756077 ) ) ;
#10140 = CARTESIAN_POINT ( 'NONE',  ( -1.005545769327274827E-13, 2.180000000000013483, -13.50000000000000000 ) ) ;
#10141 = CARTESIAN_POINT ( 'NONE',  ( -8.043339635996304082, -32.29374999999990337, -8.043339635997652337 ) ) ;
#10142 = CIRCLE ( 'NONE', #8461, 5.000000000000000000 ) ;
#10143 = CARTESIAN_POINT ( 'NONE',  ( 2.625108261242528052, 53.77444720219749286, 13.24532092722070509 ) ) ;
#10144 = ORIENTED_EDGE ( 'NONE', *, *, #381, .F. ) ;
#10145 = CYLINDRICAL_SURFACE ( 'NONE', #14283, 26.00000000000000355 ) ;
#10146 = EDGE_LOOP ( 'NONE', ( #3227, #11615, #7929, #14762 ) ) ;
#10147 = DIRECTION ( 'NONE',  ( -0.000000000000000000, -1.000000000000000000, -0.000000000000000000 ) ) ;
#10148 = CARTESIAN_POINT ( 'NONE',  ( -5.820456496121892975, 34.39186628428911519, -12.18180719480813146 ) ) ;
#10149 = CARTESIAN_POINT ( 'NONE',  ( 8.343458848123583849, 16.87999999999999545, -11.48378591275253768 ) ) ;
#10150 = CARTESIAN_POINT ( 'NONE',  ( 8.043339635996298753, -21.81874999999996234, 8.043339635997652337 ) ) ;
#10151 = AXIS2_PLACEMENT_3D ( 'NONE', #11803, #14605, #17090 ) ;
#10152 = CARTESIAN_POINT ( 'NONE',  ( 4.704097590039896026, 77.84933813905681177, 12.65644523216417028 ) ) ;
#10153 = DIRECTION ( 'NONE',  ( 0.000000000000000000, 0.000000000000000000, -1.000000000000000000 ) ) ;
#10154 = CARTESIAN_POINT ( 'NONE',  ( 0.000000000000000000, 0.000000000000000000, 0.000000000000000000 ) ) ;
#10155 = CARTESIAN_POINT ( 'NONE',  ( -7.499999999999996447, -22.51612366527185571, -9.346045933502390213 ) ) ;
#10156 = CARTESIAN_POINT ( 'NONE',  ( 13.41671563044160642, 72.37743211696324863, 1.501316902429144839 ) ) ;
#10157 = CARTESIAN_POINT ( 'NONE',  ( 11.76794919243112325, 32.28000000000000114, 3.823638476888996163 ) ) ;
#10158 = CARTESIAN_POINT ( 'NONE',  ( -13.49999999999999822, 55.78000000000000114, -4.386415899144240349 ) ) ;
#10159 = CARTESIAN_POINT ( 'NONE',  ( -2.287575323369731795, 52.26225204508322975, -13.30505731867491903 ) ) ;
#10160 = EDGE_CURVE ( 'NONE', #9800, #11548, #17063, .T. ) ;
#10161 = CARTESIAN_POINT ( 'NONE',  ( -8.343458848123582072, 52.37999999999999545, 11.48378591275254124 ) ) ;
#10162 = CARTESIAN_POINT ( 'NONE',  ( 18.36027427702394732, 7.956016705491392393, -1.158215859972921313 ) ) ;
#10163 = AXIS2_PLACEMENT_3D ( 'NONE', #1118, #7680, #9360 ) ;
#10164 = CARTESIAN_POINT ( 'NONE',  ( 11.76794919243112325, -0.7200000000000004174, 3.823638476888996163 ) ) ;
#10165 = CARTESIAN_POINT ( 'NONE',  ( -1.124720807883521134, 68.63959828170268906, 13.45321750979929831 ) ) ;
#10166 = CARTESIAN_POINT ( 'NONE',  ( -7.714727599200467800, -11.44687499999997371, 18.62499999999934630 ) ) ;
#10167 = CARTESIAN_POINT ( 'NONE',  ( -8.343458848123578520, 4.480000000000010196, -11.48378591275254124 ) ) ;
#10168 = CARTESIAN_POINT ( 'NONE',  ( -7.714727599197335195, -38.50312499999991189, -18.62500000000064304 ) ) ;
#10169 = CARTESIAN_POINT ( 'NONE',  ( -5.188624757180122060, 65.49247307178023902, 12.46307245499054517 ) ) ;
#10170 = CARTESIAN_POINT ( 'NONE',  ( -8.891200544363830713E-16, 7.546025403784439867, 12.00000000000000000 ) ) ;
#10171 = CARTESIAN_POINT ( 'NONE',  ( -2.138190042150991399, 3.603118574164297261, 13.49999996823268233 ) ) ;
#10172 = CARTESIAN_POINT ( 'NONE',  ( 8.343458848123578520, 24.98000000000000398, 11.48378591275254124 ) ) ;
#10173 = ORIENTED_EDGE ( 'NONE', *, *, #1224, .T. ) ;
#10174 = CARTESIAN_POINT ( 'NONE',  ( 11.76794919243112680, 37.58000000000000540, -3.823638476888993942 ) ) ;
#10175 = CARTESIAN_POINT ( 'NONE',  ( -3.168841352280721502, 40.29393185182132697, -13.12324853033191374 ) ) ;
#10176 = CARTESIAN_POINT ( 'NONE',  ( -13.02011563133146765, 31.80264107109495697, -3.568385494409815450 ) ) ;
#10177 = CARTESIAN_POINT ( 'NONE',  ( 3.677119991341980754, 74.81221565746179181, 12.98956592640999830 ) ) ;
#10178 = CARTESIAN_POINT ( 'NONE',  ( 13.50000000000000355, 3.580000000000008953, -4.386415899144233244 ) ) ;
#10179 = CARTESIAN_POINT ( 'NONE',  ( 2.607531440858944223E-15, 84.17999999999999261, -14.19474002721660355 ) ) ;
#10180 = CARTESIAN_POINT ( 'NONE',  ( 12.63933979188332479, 51.60176062895381932, -4.743111560129607440 ) ) ;
#10181 = CARTESIAN_POINT ( 'NONE',  ( -13.49989394954305588, 37.94506420804570013, 0.4415588883962403011 ) ) ;
#10182 = CARTESIAN_POINT ( 'NONE',  ( 8.534433506530605840, 36.85283109795096834, -10.46091794006641074 ) ) ;
#10183 = CARTESIAN_POINT ( 'NONE',  ( 8.043339635996298753, -21.81874999999996234, 8.043339635997652337 ) ) ;
#10184 = CARTESIAN_POINT ( 'NONE',  ( -0.009181258512500184085, 49.18033011924610776, -13.49999765788927064 ) ) ;
#10185 = CARTESIAN_POINT ( 'NONE',  ( -4.319557087832021303, 80.52465274632413639, 12.79068498944547905 ) ) ;
#10186 = CARTESIAN_POINT ( 'NONE',  ( 13.49542268721398486, 48.41792802572773979, 0.3515307404469304453 ) ) ;
#10187 = CARTESIAN_POINT ( 'NONE',  ( -3.636496289402152637, 12.33000000000000718, -11.19198476289190936 ) ) ;
#10188 = EDGE_CURVE ( 'NONE', #1191, #7389, #16169, .T. ) ;
#10189 = EDGE_LOOP ( 'NONE', ( #12512, #16305 ) ) ;
#10190 = CARTESIAN_POINT ( 'NONE',  ( 7.272992578804308828, 63.97999999999999687, 10.01041549318726886 ) ) ;
#10191 = CARTESIAN_POINT ( 'NONE',  ( 7.714727599197340524, -89.52812499999977547, 18.62500000000063949 ) ) ;
#10192 = CARTESIAN_POINT ( 'NONE',  ( -12.50000000000000000, 98.93000000000002103, 1.224646799147353059E-15 ) ) ;
#10193 = CARTESIAN_POINT ( 'NONE',  ( -13.50000000000000000, -1.069999999999987628, -3.469446951953614189E-15 ) ) ;
#10194 = CARTESIAN_POINT ( 'NONE',  ( -11.76794919243112325, 30.93000000000001393, -2.602085213965210642E-15 ) ) ;
#10195 = CARTESIAN_POINT ( 'NONE',  ( 3.184420153851656110, 76.06550818570755723, -13.12039170739967098 ) ) ;
#10196 = CARTESIAN_POINT ( 'NONE',  ( -7.714727599200466912, -28.09687499999992966, 18.62499999999934985 ) ) ;
#10197 = CARTESIAN_POINT ( 'NONE',  ( 4.412288822437548497, 65.83840567029228907, 12.76607370684300236 ) ) ;
#10198 = AXIS2_PLACEMENT_3D ( 'NONE', #7048, #15314, #11017 ) ;
#10199 = CARTESIAN_POINT ( 'NONE',  ( 13.50000000000000355, 81.57999999999998408, -4.386415899144233244 ) ) ;
#10200 = CARTESIAN_POINT ( 'NONE',  ( 11.76794919243112325, 46.42999999999999972, 1.441158131103945434E-15 ) ) ;
#10201 = CARTESIAN_POINT ( 'NONE',  ( -11.06704697272087579, 59.22141069247929579, 7.731141691505153624 ) ) ;
#10202 = CARTESIAN_POINT ( 'NONE',  ( 12.98058781010997009, 45.29739780767026502, 3.708848460215144804 ) ) ;
#10203 = CARTESIAN_POINT ( 'NONE',  ( 9.404160778349385907, 69.81134698545751860, -9.693570510553916719 ) ) ;
#10204 = CARTESIAN_POINT ( 'NONE',  ( 4.822590792482460920, 80.85373989299547759, 12.61238363178463118 ) ) ;
#10205 = CARTESIAN_POINT ( 'NONE',  ( 13.47269901431903705, 30.46011270062681575, -0.8715263847070852110 ) ) ;
#10206 = CARTESIAN_POINT ( 'NONE',  ( -10.91251700311249984, 56.23059369663675255, 7.948489508437808659 ) ) ;
#10207 = CARTESIAN_POINT ( 'NONE',  ( -3.918493925263932809, 50.53910349840194272, 12.91881581933787615 ) ) ;
#10208 = CARTESIAN_POINT ( 'NONE',  ( -12.50000000000000000, -22.00000000000000355, -1.714505518806294835E-15 ) ) ;
#10209 = DIRECTION ( 'NONE',  ( 0.000000000000000000, 0.000000000000000000, 1.000000000000000000 ) ) ;
#10210 = CARTESIAN_POINT ( 'NONE',  ( 11.11374454754978203, 39.71854023908382914, -7.664195384031204483 ) ) ;
#10211 = ORIENTED_EDGE ( 'NONE', *, *, #1885, .F. ) ;
#10212 = CARTESIAN_POINT ( 'NONE',  ( -13.41912378192338906, 61.98242377346405618, 1.505696609645044370 ) ) ;
#10213 = EDGE_LOOP ( 'NONE', ( #4985, #1249, #16263, #13471 ) ) ;
#10214 = ORIENTED_EDGE ( 'NONE', *, *, #848, .F. ) ;
#10215 = CARTESIAN_POINT ( 'NONE',  ( 13.49999999999999822, 33.28000000000002245, 4.386415899144237684 ) ) ;
#10216 = CARTESIAN_POINT ( 'NONE',  ( 7.714727599197338748, -30.17812499999993747, 18.62500000000063949 ) ) ;
#10217 = CARTESIAN_POINT ( 'NONE',  ( 11.64509123620695341, 48.17585162153407197, 6.829551714163834220 ) ) ;
#10218 = CARTESIAN_POINT ( 'NONE',  ( 5.350032676027314693, 57.98638694014967143, -12.39911101267510141 ) ) ;
#10219 = CARTESIAN_POINT ( 'NONE',  ( 10.87629897145368929, 78.73263608150857351, -7.997304871519990144 ) ) ;
#10220 = CARTESIAN_POINT ( 'NONE',  ( -9.520470885617717371, 81.22999999999998977, 6.917026985038133624 ) ) ;
#10221 = CARTESIAN_POINT ( 'NONE',  ( 13.49999999999999822, 38.27999999999999403, 4.386415899144237684 ) ) ;
#10222 = DIRECTION ( 'NONE',  ( -1.000000000000000000, -0.000000000000000000, -0.000000000000000000 ) ) ;
#10223 = CYLINDRICAL_SURFACE ( 'NONE', #10707, 13.50000000000000000 ) ;
#10224 = PLANE ( 'NONE',  #4298 ) ;
#10225 = CARTESIAN_POINT ( 'NONE',  ( -11.37500000000000178, -34.37499999999990052, -9.545674412382054647E-13 ) ) ;
#10226 = CARTESIAN_POINT ( 'NONE',  ( -8.891200544363830713E-16, 79.67999999999999261, 13.50000000000000000 ) ) ;
#10227 = CARTESIAN_POINT ( 'NONE',  ( 2.848479376167694532, 34.07758484385156095, -13.19633634240523001 ) ) ;
#10228 = VERTEX_POINT ( 'NONE', #1661 ) ;
#10229 = CARTESIAN_POINT ( 'NONE',  ( 0.000000000000000000, 0.000000000000000000, 0.000000000000000000 ) ) ;
#10230 = EDGE_CURVE ( 'NONE', #11897, #4019, #7387, .T. ) ;
#10231 = VERTEX_POINT ( 'NONE', #15605 ) ;
#10232 = AXIS2_PLACEMENT_3D ( 'NONE', #4772, #3351, #11493 ) ;
#10233 = CARTESIAN_POINT ( 'NONE',  ( 2.692306382202049431, 67.08319488902810690, -13.22882663213062848 ) ) ;
#10234 = CARTESIAN_POINT ( 'NONE',  ( -11.37500000000039613, -33.26562499999994316, 4.711679271993000739 ) ) ;
#10235 = DIRECTION ( 'NONE',  ( 0.000000000000000000, 0.000000000000000000, 1.000000000000000000 ) ) ;
#10236 = CARTESIAN_POINT ( 'NONE',  ( -6.070109238205766644, 59.45833234045775839, 12.06637233067175785 ) ) ;
#10237 = DIRECTION ( 'NONE',  ( 4.676985943005715098E-16, 0.000000000000000000, 1.000000000000000000 ) ) ;
#10238 = CARTESIAN_POINT ( 'NONE',  ( 17.32050807568879236, 0.000000000000000000, -9.999999999999960920 ) ) ;
#10239 = CARTESIAN_POINT ( 'NONE',  ( 12.02390709123288026, 72.65644516203032310, -6.142304361847497951 ) ) ;
#10240 = CARTESIAN_POINT ( 'NONE',  ( -7.409984580736203970E-16, 31.68000000000000682, 12.37355403259654985 ) ) ;
#10241 = CARTESIAN_POINT ( 'NONE',  ( 10.92172942406179104, 51.72999999999999687, -7.935100905948385908 ) ) ;
#10242 = CARTESIAN_POINT ( 'NONE',  ( -8.866856944732615986, 52.52278280499852059, -10.17986386199988402 ) ) ;
#10243 = VECTOR ( 'NONE', #11151, 1000.000000000000000 ) ;
#10244 = CARTESIAN_POINT ( 'NONE',  ( 11.37500000000000000, -99.89999999999976410, 0.000000000000000000 ) ) ;
#10245 = CARTESIAN_POINT ( 'NONE',  ( -7.714727599200467800, -61.39687499999984510, 18.62499999999934630 ) ) ;
#10246 = CARTESIAN_POINT ( 'NONE',  ( -8.579405063118292318, 68.35072221898208511, 10.42323635129704229 ) ) ;
#10247 = CARTESIAN_POINT ( 'NONE',  ( -13.16986379960055231, -27.05624999999993463, 13.16986379959834252 ) ) ;
#10248 = CARTESIAN_POINT ( 'NONE',  ( 0.000000000000000000, 80.93000000000000682, 0.000000000000000000 ) ) ;
#10249 = CARTESIAN_POINT ( 'NONE',  ( -7.714727599200467800, -11.44687499999997371, 18.62499999999934630 ) ) ;
#10250 = CARTESIAN_POINT ( 'NONE',  ( -5.186584049524258333, 65.49254861102842540, 12.46392224160446283 ) ) ;
#10251 = CARTESIAN_POINT ( 'NONE',  ( 15.28534784291402993, 6.548267719634617734, -18.06260399879745293 ) ) ;
#10252 = DIRECTION ( 'NONE',  ( 0.000000000000000000, -1.000000000000000000, 0.000000000000000000 ) ) ;
#10253 = ORIENTED_EDGE ( 'NONE', *, *, #5724, .F. ) ;
#10254 = LINE ( 'NONE', #13152, #17451 ) ;
#10255 = CARTESIAN_POINT ( 'NONE',  ( -17.42428528562871293, 5.918584287042171432, 19.29752010712834220 ) ) ;
#10256 = CARTESIAN_POINT ( 'NONE',  ( -2.805409333583691378, 40.28087191790951493, -13.20536015821407361 ) ) ;
#10257 = AXIS2_PLACEMENT_3D ( 'NONE', #17139, #3800, #14564 ) ;
#10258 = CARTESIAN_POINT ( 'NONE',  ( -13.12180246013672757, 31.81716720392802600, -3.176623397036585583 ) ) ;
#10259 = CARTESIAN_POINT ( 'NONE',  ( 1.324652792791208178, 74.72762950812426652, 13.43485395247348180 ) ) ;
#10260 = CARTESIAN_POINT ( 'NONE',  ( 9.404743306317577378, 60.04888379170549229, 9.685242053972840992 ) ) ;
#10261 = CARTESIAN_POINT ( 'NONE',  ( 11.02516507505776211, -4.913438141677136737E-17, -3.106252184828564467 ) ) ;
#10262 = SHAPE_REPRESENTATION_RELATIONSHIP ( 'NONE' , 'NONE' ,  #8052, #15536 ) ;
#10263 = CARTESIAN_POINT ( 'NONE',  ( -8.691771469529815392E-16, 76.68000000000000682, 14.19474002721660355 ) ) ;
#10264 = CARTESIAN_POINT ( 'NONE',  ( 13.23825292412364263, 51.52337512777393158, -2.645500850496228296 ) ) ;
#10265 = CARTESIAN_POINT ( 'NONE',  ( -11.19854509087375760, 38.21339351073512347, 7.539409783578506108 ) ) ;
#10266 = CARTESIAN_POINT ( 'NONE',  ( 11.24391244297007120, 36.71057840753311297, -7.471579428428752223 ) ) ;
#10267 = CARTESIAN_POINT ( 'NONE',  ( 11.37499999999999645, -23.89999999999996305, 9.531744055041752924E-13 ) ) ;
#10268 = DIRECTION ( 'NONE',  ( 0.000000000000000000, -1.000000000000000000, 0.000000000000000000 ) ) ;
#10269 = CARTESIAN_POINT ( 'NONE',  ( -6.693563675217492737, 77.43309452535775961, 11.72466887716232975 ) ) ;
#10270 = EDGE_CURVE ( 'NONE', #9130, #908, #12120, .T. ) ;
#10271 = CARTESIAN_POINT ( 'NONE',  ( -4.171729424061787483, 60.32999999999999829, -12.83926296998457417 ) ) ;
#10272 = CARTESIAN_POINT ( 'NONE',  ( 5.983495836244371091, 41.89831291724665618, 12.10301303378507853 ) ) ;
#10273 = CARTESIAN_POINT ( 'NONE',  ( 12.15164001199787869, 48.64617462453512076, -5.883719564323237172 ) ) ;
#10274 = CARTESIAN_POINT ( 'NONE',  ( -11.76794919243112325, 16.08000000000000895, 3.823638476888994386 ) ) ;
#10275 = ORIENTED_EDGE ( 'NONE', *, *, #12615, .F. ) ;
#10276 = CARTESIAN_POINT ( 'NONE',  ( -7.272992578804307939, 59.48000000000000398, -10.01041549318727064 ) ) ;
#10277 = CARTESIAN_POINT ( 'NONE',  ( 18.62500000000000000, -75.99999999999980105, 1.560692158462880521E-12 ) ) ;
#10278 = CARTESIAN_POINT ( 'NONE',  ( -15.58845726811976817, 0.000000000000000000, -11.00000000000018296 ) ) ;
#10279 = CARTESIAN_POINT ( 'NONE',  ( 13.50000000000000355, -2.420000000000005258, -4.386415899144233244 ) ) ;
#10280 = CARTESIAN_POINT ( 'NONE',  ( -3.636496289402156190, 31.53000000000000114, 11.19198476289190758 ) ) ;
#10281 = CARTESIAN_POINT ( 'NONE',  ( -8.000000000000177636, 6.548282979925672542, 22.26874168100108875 ) ) ;
#10282 = CARTESIAN_POINT ( 'NONE',  ( 18.62500000000000000, -66.59999999999983800, 1.560692158462880521E-12 ) ) ;
#10283 = CARTESIAN_POINT ( 'NONE',  ( 8.343458848123578520, 77.97999999999998977, 11.48378591275254124 ) ) ;
#10284 = CARTESIAN_POINT ( 'NONE',  ( 7.272992578804311492, 46.87999999999998835, -10.01041549318726709 ) ) ;
#10285 = CARTESIAN_POINT ( 'NONE',  ( -11.48042453290631215, 9.879967940401300552, -4.614170634023106565 ) ) ;
#10286 = CARTESIAN_POINT ( 'NONE',  ( -10.69285981900389082, 59.24332124397713528, 8.245168519117006767 ) ) ;
#10287 = CARTESIAN_POINT ( 'NONE',  ( 11.29577473244720132, 45.15263884231691094, 7.394358328561038363 ) ) ;
#10288 = CARTESIAN_POINT ( 'NONE',  ( 1.102632182866101207, 70.14042570178519043, -13.45669853540183425 ) ) ;
#10289 = CARTESIAN_POINT ( 'NONE',  ( 0.7449732705081377748, 80.70681811148803320, 13.48519498389669735 ) ) ;
#10290 = CARTESIAN_POINT ( 'NONE',  ( 13.31353121000146444, 30.35142671438330098, 2.236827078041004224 ) ) ;
#10291 = CARTESIAN_POINT ( 'NONE',  ( -13.46326036990713249, 55.96444472986166119, 0.9953224451197258960 ) ) ;
#10292 = CARTESIAN_POINT ( 'NONE',  ( -13.47134942828595427, 49.96064118497289286, 0.8867589712405034019 ) ) ;
#10293 = CARTESIAN_POINT ( 'NONE',  ( 5.649316163632027710, 63.97492181549525725, -12.26175092916859732 ) ) ;
#10294 = CARTESIAN_POINT ( 'NONE',  ( 2.905705795190346219, 43.07552160509550987, -13.18358388524940317 ) ) ;
#10295 = CARTESIAN_POINT ( 'NONE',  ( 11.96927535954811006, 39.66052931784707170, -6.243969760129989055 ) ) ;
#10296 = EDGE_LOOP ( 'NONE', ( #11357, #13024, #5804, #4918 ) ) ;
#10297 = CARTESIAN_POINT ( 'NONE',  ( -12.02744370554971276, 61.70390941226424530, -6.131723170855442717 ) ) ;
#10298 = ORIENTED_EDGE ( 'NONE', *, *, #17466, .F. ) ;
#10299 = ORIENTED_EDGE ( 'NONE', *, *, #11299, .F. ) ;
#10300 = CARTESIAN_POINT ( 'NONE',  ( 13.50000000000000000, 30.43000000000001393, 1.734723475976807094E-15 ) ) ;
#10301 = CARTESIAN_POINT ( 'NONE',  ( 7.714727599197340524, -104.0281249999997755, 18.62500000000063949 ) ) ;
#10302 = CARTESIAN_POINT ( 'NONE',  ( 11.88874087135845237, 48.19328206360869160, 6.400001648777170260 ) ) ;
#10303 = CARTESIAN_POINT ( 'NONE',  ( 6.489056890134116351, 57.94152136233466877, -11.84633360268247060 ) ) ;
#10304 = CARTESIAN_POINT ( 'NONE',  ( 11.65723228743481776, 78.68382482704133452, -6.824437818837509440 ) ) ;
#10305 = CARTESIAN_POINT ( 'NONE',  ( -7.272992578804307939, 74.47999999999998977, -10.01041549318726886 ) ) ;
#10306 = CARTESIAN_POINT ( 'NONE',  ( 11.54774696664502009, -1.688490311990082769E-15, 6.357251958165095473 ) ) ;
#10307 = CARTESIAN_POINT ( 'NONE',  ( 13.50000000000000355, 1.579999999999999405, -4.386415899144233244 ) ) ;
#10308 = ADVANCED_FACE ( 'NONE', ( #15781 ), #7596, .T. ) ;
#10309 = CLOSED_SHELL ( 'NONE', ( #9079, #9479, #7916, #6652, #11622, #2652, #9298, #2266, #5808, #6046, #16371, #7438, #12090, #16671, #11862, #12950, #7137, #5708, #14210, #8502, #16138, #8255, #455, #10776 ) ) ;
#10310 = CARTESIAN_POINT ( 'NONE',  ( -0.3664410078159376360, 67.19317488031707342, -13.49530529745837448 ) ) ;
#10311 = CARTESIAN_POINT ( 'NONE',  ( -8.043339635997654113, -36.45624999999989768, 8.043339635996304082 ) ) ;
#10312 = DIRECTION ( 'NONE',  ( -0.000000000000000000, -1.000000000000000000, -0.000000000000000000 ) ) ;
#10313 = CARTESIAN_POINT ( 'NONE',  ( 5.813126995088480520, 33.96841089008475478, -12.18431645958717979 ) ) ;
#10314 = ORIENTED_EDGE ( 'NONE', *, *, #7675, .T. ) ;
#10315 = CARTESIAN_POINT ( 'NONE',  ( 8.375056734751542109, 9.999950376471138824, 10.58801762894534271 ) ) ;
#10316 = EDGE_LOOP ( 'NONE', ( #7388, #4900, #1598, #11813, #17294, #8106 ) ) ;
#10317 = CARTESIAN_POINT ( 'NONE',  ( 2.747298874549415793, 67.08121722534593800, -13.21751473180457026 ) ) ;
#10318 = CARTESIAN_POINT ( 'NONE',  ( -4.711679271994915652, -35.34687499999993321, 11.37499999999960210 ) ) ;
#10319 = CARTESIAN_POINT ( 'NONE',  ( 8.655293140891854975, 78.01281519178354529, 10.36031341550661899 ) ) ;
#10320 = CARTESIAN_POINT ( 'NONE',  ( -17.32050807568865736, 0.000000000000000000, -10.00000000000020428 ) ) ;
#10321 = LINE ( 'NONE', #15676, #1560 ) ;
#10322 = CARTESIAN_POINT ( 'NONE',  ( 7.347880794884121708E-16, 102.9300000000000068, -6.000000000000001776 ) ) ;
#10323 = CYLINDRICAL_SURFACE ( 'NONE', #14426, 12.00000000000000178 ) ;
#10324 =( BOUNDED_CURVE ( )  B_SPLINE_CURVE ( 2, ( #100, #5330, #5157, #4074, #10802, #15909, #13354, #12036, #3818, #12119, #17333, #16164, #17415 ),
 .UNSPECIFIED., .F., .F. ) 
 B_SPLINE_CURVE_WITH_KNOTS ( ( 3, 2, 2, 2, 2, 2, 3 ),
 ( 0.1297968370382597270, 0.1335521526262006542, 0.1410627838020607483, 0.1485734149779206759, 0.1560840461537806034, 0.1635946773296405587, 0.1673499929175705225 ),
 .UNSPECIFIED. ) 
 CURVE ( )  GEOMETRIC_REPRESENTATION_ITEM ( )  RATIONAL_B_SPLINE_CURVE ( ( 0.9755282581475767101, 0.9755282581475053227, 1.000000000000000000, 0.9510565162951534202, 1.000000000000000000, 0.9510565162951534202, 1.000000000000000000, 0.9510565162951534202, 1.000000000000000000, 0.9510565162951534202, 1.000000000000000000, 0.9755282581475767101, 0.9755282581475767101 ) ) 
 REPRESENTATION_ITEM ( '' )  );
#10325 = CARTESIAN_POINT ( 'NONE',  ( -13.49999999999999822, 50.07999999999999119, 4.386415899144235908 ) ) ;
#10326 = CARTESIAN_POINT ( 'NONE',  ( -10.79414870313322083, 71.23842559514402240, 8.155184730919005531 ) ) ;
#10327 = EDGE_CURVE ( 'NONE', #368, #3099, #4680, .T. ) ;
#10328 = B_SPLINE_CURVE_WITH_KNOTS ( 'NONE', 3,
 ( #4693, #13776, #1675, #7090, #12474, #13861, #5766, #3174, #12644, #8598, #11150, #1847, #620, #14128, #16526, #16701, #11415, #15186, #6032, #8684, #4433, #14043, #8513, #448, #7260, #1765, #2015, #7174, #10098, #5858, #12383, #4606, #10012, #274, #12562, #533, #5685, #15448, #10182, #11757, #4863, #15533, #9206, #6373, #11498, #10440, #6118, #15799, #14558, #16874, #14299, #708, #15618, #3526, #7442, #5132, #961, #10266, #3704, #15886, #7525, #14213, #4779, #7613, #3794, #1050, #17133, #3444, #12821, #16961, #5043, #8861, #4952, #2098, #12905, #11847, #6199, #789, #8941, #10355, #9121, #14383, #11585, #2185, #12989, #17222, #13075, #872, #14471, #15709, #7698, #6283, #11671, #17046, #3613, #2359, #9027, #2272, #7792, #13163, #6462, #10523, #17394, #1483, #2707, #2533, #1304, #1137, #14728, #8136, #10957, #2617, #9643, #14903, #7961, #6548, #5481, #2797, #11927, #13250, #17308, #8047, #5310, #16231, #13331, #8228, #10693, #16059, #7873, #15974, #3967, #14645, #13589, #3877, #76, #9465, #9379, #5221, #6635, #1222, #12014, #10607, #9293, #13414, #6718, #12096, #17478, #13501, #5392, #10777, #14812, #6900, #4232, #16141, #1391, #12273, #4051, #9553, #10863, #6806, #12184, #4140, #170, #5575, #16325, #2441, #12456, #11303, #8493, #4914, #7241, #13931, #2885, #13757, #11133, #8317 ),
 .UNSPECIFIED., .F., .F.,
 ( 4, 2, 2, 2, 1, 1, 1, 2, 2, 2, 1, 1, 1, 1, 2, 2, 2, 2, 2, 1, 1, 2, 2, 1, 2, 2, 2, 2, 1, 2, 2, 1, 2, 2, 2, 1, 1, 2, 2, 2, 1, 1, 2, 2, 2, 2, 2, 2, 2, 1, 2, 2, 1, 2, 2, 2, 2, 2, 2, 1, 2, 2, 2, 2, 1, 1, 1, 2, 2, 2, 2, 2, 2, 2, 2, 2, 1, 2, 2, 2, 1, 1, 2, 2, 1, 2, 2, 2, 2, 2, 1, 1, 2, 2, 1, 2, 2, 2, 1, 1, 1, 2, 2, 4 ),
 ( 0.8578524185686006165, 0.8579098628542002336, 0.8579242239256001934, 0.8579385849970000422, 0.8579673071397998507, 0.8580821957109991960, 0.8583119728533977755, 0.8587715271381948234, 0.8596906357077890304, 0.8615288528469774443, 0.8617586299893760238, 0.8618735185605752580, 0.8619309628461748751, 0.8619596849889746837, 0.8619740460603746435, 0.8619884071317744922, 0.8624479614165716512, 0.8633670699861659692, 0.8638266242709631282, 0.8639415128421624734, 0.8639989571277620906, 0.8640133181991619393, 0.8640276792705618991, 0.8640564014133617077, 0.8642861785557602872, 0.8652052871253544941, 0.8656648414101516531, 0.8658946185525502326, 0.8660095071237494668, 0.8660382292665492754, 0.8660669514093491950, 0.8661243956949488121, 0.8670435042645431301, 0.8670578653359429788, 0.8670722264073429386, 0.8671009485501427472, 0.8671583928357423643, 0.8672732814069417095, 0.8675030585493402890, 0.8679626128341374480, 0.8680200571197371762, 0.8680487792625369847, 0.8680631403339368335, 0.8680775014053367933, 0.8681923899765360275, 0.8684221671189346070, 0.8688817214037318770, 0.8698008299733261950, 0.8700306071157247745, 0.8700880514013243916, 0.8701024124727243514, 0.8701167735441242002, 0.8701454956869240087, 0.8702603842581233540, 0.8707199385429205130, 0.8716390471125148309, 0.8720986013973119899, 0.8721273235401117985, 0.8721560456829116070, 0.8722134899685113352, 0.8723283785397105694, 0.8725581556821091489, 0.8734772642517034669, 0.8739368185365007369, 0.8740517071076999711, 0.8741091513932995882, 0.8741378735360993968, 0.8741522346074993566, 0.8741665956788993164, 0.8743963728212978959, 0.8753154813908922138, 0.8757750356756893728, 0.8762345899604866428, 0.8780728070996752788, 0.8781876956708746240, 0.8782451399564742411, 0.8783025842420739693, 0.8785323613844725488, 0.8789919156692697078, 0.8799110242388641367, 0.8801408013812627162, 0.8801982456668623334, 0.8802269678096622529, 0.8802556899524620615, 0.8803705785236612957, 0.8808301328084585657, 0.8817492413780528837, 0.8822087956628501537, 0.8826683499476473127, 0.8835874585172417417, 0.8840470128020390117, 0.8842767899444375912, 0.8843055120872373998, 0.8843342342300372083, 0.8843916785156368254, 0.8845065670868361707, 0.8854256756564305997, 0.8858852299412278697, 0.8861150070836264492, 0.8862298956548257944, 0.8862873399404254116, 0.8863160620832253311, 0.8863447842260251397, 0.8872638927956195687 ),
 .UNSPECIFIED. ) ;
#10329 = CARTESIAN_POINT ( 'NONE',  ( 18.35881383260823441, 7.956441918454667750, 1.156263389813445341 ) ) ;
#10330 = CARTESIAN_POINT ( 'NONE',  ( 7.714727599200458030, -69.72187499999982663, -18.62499999999934985 ) ) ;
#10331 = CARTESIAN_POINT ( 'NONE',  ( -2.066879295991422616, 68.60558311925369424, 13.34776454378817512 ) ) ;
#10332 = CARTESIAN_POINT ( 'NONE',  ( -7.714727599197335195, -71.80312499999982379, -18.62500000000064304 ) ) ;
#10333 = CARTESIAN_POINT ( 'NONE',  ( 2.992242805631164515, 55.07242087184739887, -13.16446483759825625 ) ) ;
#10334 = CARTESIAN_POINT ( 'NONE',  ( -18.62500000000000000, -58.27499999999986358, -1.562973063126292555E-12 ) ) ;
#10335 = CARTESIAN_POINT ( 'NONE',  ( -7.707562987937823351, 65.39003898384051183, 11.08354747542285956 ) ) ;
#10336 = CARTESIAN_POINT ( 'NONE',  ( 11.00000000000001599, 7.773118517290098062, -15.58845726811988364 ) ) ;
#10337 = CARTESIAN_POINT ( 'NONE',  ( -1.595484067438319942, 35.62263446958586144, 13.40538992109765282 ) ) ;
#10338 = CARTESIAN_POINT ( 'NONE',  ( -8.549982208541774191E-16, 27.68000000000000327, 14.19474002721660355 ) ) ;
#10339 = CARTESIAN_POINT ( 'NONE',  ( 3.636496289402157078, 32.02999999999999403, -11.19198476289190936 ) ) ;
#10340 = AXIS2_PLACEMENT_3D ( 'NONE', #7810, #3546, #6393 ) ;
#10341 = CARTESIAN_POINT ( 'NONE',  ( 0.000000000000000000, 9.000000000000000000, 0.000000000000000000 ) ) ;
#10342 = CARTESIAN_POINT ( 'NONE',  ( 13.49999999999999822, 80.28000000000000114, 4.386415899144236796 ) ) ;
#10343 = CARTESIAN_POINT ( 'NONE',  ( -13.50004520387097173, 31.92232117734513608, -0.2162762051120299955 ) ) ;
#10344 = CARTESIAN_POINT ( 'NONE',  ( 0.000000000000000000, 0.000000000000000000, 0.000000000000000000 ) ) ;
#10345 = CARTESIAN_POINT ( 'NONE',  ( 11.62435398580979751, 60.17441760321225530, 6.864763562681197584 ) ) ;
#10346 = CARTESIAN_POINT ( 'NONE',  ( -8.343458848123582072, -2.620000000000006324, 11.48378591275254124 ) ) ;
#10347 = CARTESIAN_POINT ( 'NONE',  ( 4.171729424061791924, 63.03000000000000114, -12.83926296998457239 ) ) ;
#10348 = CARTESIAN_POINT ( 'NONE',  ( -9.520470885617715595, 56.63000000000000256, -6.917026985038136289 ) ) ;
#10349 = DIRECTION ( 'NONE',  ( 0.5234639319314094985, -2.026423598025616117E-25, -0.8520478343185368120 ) ) ;
#10350 = CARTESIAN_POINT ( 'NONE',  ( -8.343458848123582072, 76.37999999999998124, 11.48378591275254124 ) ) ;
#10351 = ADVANCED_FACE ( 'NONE', ( #856 ), #15691, .T. ) ;
#10352 = CARTESIAN_POINT ( 'NONE',  ( 13.44076158601913029, 51.38538528069671685, 1.282844352539189936 ) ) ;
#10353 = AXIS2_PLACEMENT_3D ( 'NONE', #7354, #15274, #9749 ) ;
#10354 = CARTESIAN_POINT ( 'NONE',  ( -13.33448719118932146, 38.00391057290926256, 2.107558467510691980 ) ) ;
#10355 = CARTESIAN_POINT ( 'NONE',  ( 12.89750109184049975, 36.57316622584918520, -3.991296069496922172 ) ) ;
#10356 = CARTESIAN_POINT ( 'NONE',  ( -9.552639591052204498E-13, -69.68749999999984368, 11.37499999999999645 ) ) ;
#10357 = CARTESIAN_POINT ( 'NONE',  ( -5.262387905378953512, 74.48968593636273283, 12.43211883244449112 ) ) ;
#10358 = CARTESIAN_POINT ( 'NONE',  ( -7.312194298746915067, 77.40724852587138116, 11.35038802565898486 ) ) ;
#10359 = CARTESIAN_POINT ( 'NONE',  ( -4.130858764561470053, 80.53146975156121812, 12.85259012924355915 ) ) ;
#10360 = CARTESIAN_POINT ( 'NONE',  ( -8.891200544363830713E-16, 5.680000000000002380, 13.49999999999999822 ) ) ;
#10361 = EDGE_LOOP ( 'NONE', ( #7910, #11202, #6704, #9324, #16838 ) ) ;
#10362 = CARTESIAN_POINT ( 'NONE',  ( -11.76794919243112325, 13.07999999999999829, 3.823638476888994386 ) ) ;
#10363 = EDGE_LOOP ( 'NONE', ( #15286, #3393, #9432, #4613 ) ) ;
#10364 = CARTESIAN_POINT ( 'NONE',  ( -11.76794919243112325, 56.92999999999999972, -2.882316262207890869E-15 ) ) ;
#10365 = CARTESIAN_POINT ( 'NONE',  ( -9.552639591052204498E-13, -55.18749999999985079, 11.37500000000000178 ) ) ;
#10366 = DIRECTION ( 'NONE',  ( -0.000000000000000000, 1.000000000000000000, -0.000000000000000000 ) ) ;
#10367 = CARTESIAN_POINT ( 'NONE',  ( 13.50000000000000000, 0.4300000000000137046, 1.734723475976807094E-15 ) ) ;
#10368 = CARTESIAN_POINT ( 'NONE',  ( 13.03682526262544350, 75.55504566543577027, -3.506206262213893421 ) ) ;
#10369 = CARTESIAN_POINT ( 'NONE',  ( -18.62500000000000000, -58.27499999999986358, -1.562973063126292555E-12 ) ) ;
#10370 = CARTESIAN_POINT ( 'NONE',  ( -4.171729424061791036, 80.53000000000000114, 12.83926296998457239 ) ) ;
#10371 = CARTESIAN_POINT ( 'NONE',  ( 11.76794919243112325, 49.28000000000000114, 3.823638476888996607 ) ) ;
#10372 = EDGE_CURVE ( 'NONE', #11076, #7647, #14116, .T. ) ;
#10373 = CARTESIAN_POINT ( 'NONE',  ( -10.01465321359413885, 59.28001650100842568, 9.053085426433254312 ) ) ;
#10374 = CARTESIAN_POINT ( 'NONE',  ( 13.49235683156874721, 45.41405812888587690, 0.4636627382355369420 ) ) ;
#10375 = CARTESIAN_POINT ( 'NONE',  ( 13.17044722332754780, 69.32228747003190961, 3.042193921996489969 ) ) ;
#10376 = CARTESIAN_POINT ( 'NONE',  ( -4.171729424061791036, 67.53000000000000114, 12.83926296998457239 ) ) ;
#10377 = CARTESIAN_POINT ( 'NONE',  ( 13.03052044818961441, 30.55590990951756325, -3.529457494173335874 ) ) ;
#10378 = CARTESIAN_POINT ( 'NONE',  ( -10.81241192308180921, 55.62348906932676584, -8.085305829502456021 ) ) ;
#10379 = CARTESIAN_POINT ( 'NONE',  ( -5.503938361541620417, 50.48042196614674992, 12.32707990364577455 ) ) ;
#10380 = CARTESIAN_POINT ( 'NONE',  ( 0.000000000000000000, 80.93000000000000682, 0.000000000000000000 ) ) ;
#10381 = CARTESIAN_POINT ( 'NONE',  ( 4.419207061359027300, 43.02104761480173778, -12.75630134412691952 ) ) ;
#10382 = CARTESIAN_POINT ( 'NONE',  ( 13.32699551091378254, 39.35439204512613287, 2.154494870127292128 ) ) ;
#10383 = VERTEX_POINT ( 'NONE', #4847 ) ;
#10384 = CARTESIAN_POINT ( 'NONE',  ( -12.11116184202662538, 70.70858905986030152, -6.028316998684753791 ) ) ;
#10385 = CARTESIAN_POINT ( 'NONE',  ( -7.265637185492512806, 61.45088050927903112, -11.37811650908751915 ) ) ;
#10386 = CARTESIAN_POINT ( 'NONE',  ( -9.520470885617717371, 7.230000000000014637, 6.917026985038133624 ) ) ;
#10387 = ORIENTED_EDGE ( 'NONE', *, *, #3850, .F. ) ;
#10388 = CARTESIAN_POINT ( 'NONE',  ( -11.73735425733374349, 40.68227936623591745, -6.671254634659874228 ) ) ;
#10389 = ORIENTED_EDGE ( 'NONE', *, *, #15578, .T. ) ;
#10390 = CARTESIAN_POINT ( 'NONE',  ( 13.49999999999999822, 21.28000000000000469, 4.386415899144237684 ) ) ;
#10391 = CARTESIAN_POINT ( 'NONE',  ( -13.16986379959834252, -22.89374999999994387, -13.16986379960055054 ) ) ;
#10392 = CARTESIAN_POINT ( 'NONE',  ( 3.309157057342323682, 47.79898824056381557, 13.08814985599747338 ) ) ;
#10393 = CARTESIAN_POINT ( 'NONE',  ( 9.127818136977767338, 57.82506099181254910, -9.960319412006729323 ) ) ;
#10394 = CARTESIAN_POINT ( 'NONE',  ( 8.740260419149842974, 78.84333345805735860, -10.29113004058012315 ) ) ;
#10395 = CARTESIAN_POINT ( 'NONE',  ( 2.272985001014427788E-15, 77.18000000000000682, -12.37355403259654985 ) ) ;
#10396 = CARTESIAN_POINT ( 'NONE',  ( -1.003751346110120011E-07, 3.679997203684337137, 13.49999999999999822 ) ) ;
#10397 = CARTESIAN_POINT ( 'NONE',  ( 11.30201554348636783, -99.99999999999994316, 1.743143577145335854 ) ) ;
#10398 = CARTESIAN_POINT ( 'NONE',  ( -0.7917850522838131289, 67.20846528983619805, -13.47766984953646840 ) ) ;
#10399 = CARTESIAN_POINT ( 'NONE',  ( 4.711679271993006957, -56.22812499999984936, 11.37500000000039613 ) ) ;
#10400 = DIRECTION ( 'NONE',  ( 0.000000000000000000, 0.000000000000000000, 1.000000000000000000 ) ) ;
#10401 = CARTESIAN_POINT ( 'NONE',  ( 8.524601824545214868, 33.85328496813475851, -10.46893613448600568 ) ) ;
#10402 = CARTESIAN_POINT ( 'NONE',  ( -12.90183522623821766, 73.78708785609254051, -3.983866183089469715 ) ) ;
#10403 = VERTEX_POINT ( 'NONE', #11654 ) ;
#10404 = CARTESIAN_POINT ( 'NONE',  ( 12.50000000000000000, 98.93000000000002103, 1.224646799147353059E-15 ) ) ;
#10405 = ORIENTED_EDGE ( 'NONE', *, *, #11641, .T. ) ;
#10406 = CARTESIAN_POINT ( 'NONE',  ( 13.50000000000000000, 15.42999999999999972, 1.734723475976807094E-15 ) ) ;
#10407 = CARTESIAN_POINT ( 'NONE',  ( 8.043339635997652337, -9.331249999999993605, -8.043339635996302306 ) ) ;
#10408 = EDGE_CURVE ( 'NONE', #12936, #12048, #6080, .T. ) ;
#10409 = CARTESIAN_POINT ( 'NONE',  ( -1.434929399941947459, 44.62842767942802880, 13.42577741823575899 ) ) ;
#10410 = CARTESIAN_POINT ( 'NONE',  ( -7.180763499379964721, 59.41272380569992606, 11.43182607564664899 ) ) ;
#10411 = LINE ( 'NONE', #2331, #1002 ) ;
#10412 = DIRECTION ( 'NONE',  ( -0.000000000000000000, -0.000000000000000000, 1.000000000000000000 ) ) ;
#10413 = CARTESIAN_POINT ( 'NONE',  ( -8.691771469529815392E-16, 56.67999999999998550, 14.19474002721660355 ) ) ;
#10414 = CARTESIAN_POINT ( 'NONE',  ( -11.83228429192144304, 71.17079610990623451, 6.499773857208959171 ) ) ;
#10415 = CARTESIAN_POINT ( 'NONE',  ( -13.16986379960055231, -60.35624999999985363, 13.16986379959834252 ) ) ;
#10416 = CARTESIAN_POINT ( 'NONE',  ( -7.557983764346632327, 68.39670004143046356, 11.19912239775939433 ) ) ;
#10417 = CARTESIAN_POINT ( 'NONE',  ( 18.62500000000000000, -16.64999999999995950, 1.560692158462880521E-12 ) ) ;
#10418 = CARTESIAN_POINT ( 'NONE',  ( 3.289654790109945992, 55.06171615666674057, -13.09305896734488606 ) ) ;
#10419 = AXIS2_PLACEMENT_3D ( 'NONE', #8575, #4496, #15072 ) ;
#10420 = CARTESIAN_POINT ( 'NONE',  ( -13.16986379959834252, -56.19374999999985931, -13.16986379960055054 ) ) ;
#10421 = CARTESIAN_POINT ( 'NONE',  ( -9.885467538893191630, 65.28675227565267392, 9.194100240487596665 ) ) ;
#10422 = CARTESIAN_POINT ( 'NONE',  ( 0.000000000000000000, -28.00000000000000000, 0.000000000000000000 ) ) ;
#10423 = CARTESIAN_POINT ( 'NONE',  ( -4.873736741403357442, 35.50432647131191999, 12.59114714938776736 ) ) ;
#10424 = ADVANCED_FACE ( 'NONE', ( #10086 ), #2084, .F. ) ;
#10425 = ORIENTED_EDGE ( 'NONE', *, *, #12732, .T. ) ;
#10426 = DIRECTION ( 'NONE',  ( 0.000000000000000000, 0.000000000000000000, -1.000000000000000000 ) ) ;
#10427 =( BOUNDED_CURVE ( )  B_SPLINE_CURVE ( 2, ( #3216, #15229, #7212, #1886, #7130, #313, #12600, #7300, #12427, #5895, #13904, #15050, #4559 ),
 .UNSPECIFIED., .F., .F. ) 
 B_SPLINE_CURVE_WITH_KNOTS ( ( 3, 2, 2, 2, 2, 2, 3 ),
 ( 0.3472222222222222099, 0.3499999999999999778, 0.3555555555555555691, 0.3611111111111111049, 0.3666666666666666408, 0.3722222222222222321, 0.3750000000000000000 ),
 .UNSPECIFIED. ) 
 CURVE ( )  GEOMETRIC_REPRESENTATION_ITEM ( )  RATIONAL_B_SPLINE_CURVE ( ( 0.9755282581475768211, 0.9755282581475768211, 1.000000000000000000, 0.9510565162951535312, 1.000000000000000000, 0.9510565162951535312, 1.000000000000000000, 0.9510565162951535312, 1.000000000000000000, 0.9510565162951535312, 1.000000000000000000, 0.9755282581475768211, 0.9755282581475768211 ) ) 
 REPRESENTATION_ITEM ( '' )  );
#10428 = DIRECTION ( 'NONE',  ( 0.000000000000000000, -0.2588190451025143002, -0.9659258262890700886 ) ) ;
#10429 = CARTESIAN_POINT ( 'NONE',  ( -1.245860404445607248E-06, 40.18000018109674443, -13.49999999999994316 ) ) ;
#10430 = CARTESIAN_POINT ( 'NONE',  ( -13.32379211457350721, 32.00634305175220362, 2.174812285166201509 ) ) ;
#10431 = CARTESIAN_POINT ( 'NONE',  ( 17.42428528562844292, 5.918584287042172321, 19.29752010712858024 ) ) ;
#10432 = CARTESIAN_POINT ( 'NONE',  ( 12.62498755182630461, 60.25550772051544612, 4.821155371132717526 ) ) ;
#10433 = CARTESIAN_POINT ( 'NONE',  ( 8.343458848123578520, -11.02000000000000846, 11.48378591275254124 ) ) ;
#10434 = CARTESIAN_POINT ( 'NONE',  ( -10.00804607396390189, 53.28036437624847110, 9.060407765840576388 ) ) ;
#10435 = AXIS2_PLACEMENT_3D ( 'NONE', #7089, #11236, #11062 ) ;
#10436 = CARTESIAN_POINT ( 'NONE',  ( -7.576616670048093940E-16, 54.67999999999999261, 12.37355403259654985 ) ) ;
#10437 = APPLICATION_PROTOCOL_DEFINITION ( 'draft international standard', 'automotive_design', 1998, #4739 ) ;
#10438 = CARTESIAN_POINT ( 'NONE',  ( 13.39324380192281971, 51.37084852268094437, 1.694922732828999967 ) ) ;
#10439 = CARTESIAN_POINT ( 'NONE',  ( -13.47682487734259738, 37.90268679109564687, -0.7907200057638921198 ) ) ;
#10440 = CARTESIAN_POINT ( 'NONE',  ( 10.29076770525271556, 36.76532346438606424, -8.737960796721409906 ) ) ;
#10441 = CARTESIAN_POINT ( 'NONE',  ( -11.37499999999960210, -64.48437499999987210, -4.711679271994911211 ) ) ;
#10442 = CARTESIAN_POINT ( 'NONE',  ( -6.074181061366862977, 74.45811146783317724, 12.05629934353452093 ) ) ;
#10443 = CARTESIAN_POINT ( 'NONE',  ( -12.04419590223588443, 77.15471538261230933, 6.098651071946050273 ) ) ;
#10444 = CARTESIAN_POINT ( 'NONE',  ( 1.590819206443820466, 62.73723098374880891, 13.40788169120826545 ) ) ;
#10445 = CARTESIAN_POINT ( 'NONE',  ( 7.500000000000000000, 108.6686507028258575, 2.034160311361953521 ) ) ;
#10446 = ORIENTED_EDGE ( 'NONE', *, *, #4165, .F. ) ;
#10447 = AXIS2_PLACEMENT_3D ( 'NONE', #5972, #1958, #7382 ) ;
#10448 = CARTESIAN_POINT ( 'NONE',  ( 11.76794919243112680, 11.58000000000000362, -3.823638476888993942 ) ) ;
#10449 = VERTEX_POINT ( 'NONE', #14367 ) ;
#10450 = CARTESIAN_POINT ( 'NONE',  ( -3.636496289402153081, 59.32999999999999829, -11.19198476289190936 ) ) ;
#10451 = CARTESIAN_POINT ( 'NONE',  ( -11.37500000000039790, -68.71562499999981810, 4.711679271993001628 ) ) ;
#10452 = CARTESIAN_POINT ( 'NONE',  ( 12.50000000000000000, -18.00000000000000355, -2.204364238465235822E-15 ) ) ;
#10453 = CARTESIAN_POINT ( 'NONE',  ( 4.171729424061791924, -1.969999999999999529, -12.83926296998457239 ) ) ;
#10454 = EDGE_CURVE ( 'NONE', #12212, #14613, #11740, .T. ) ;
#10455 = CARTESIAN_POINT ( 'NONE',  ( 4.018767646357342294, 76.03543680882090428, -12.88819257462414392 ) ) ;
#10456 = CARTESIAN_POINT ( 'NONE',  ( -13.49999999999999822, 67.78000000000001535, -4.386415899144240349 ) ) ;
#10457 = CARTESIAN_POINT ( 'NONE',  ( -11.76794919243112325, 45.07999999999999829, 3.823638476888994386 ) ) ;
#10458 = CARTESIAN_POINT ( 'NONE',  ( 10.92172942406178926, 7.129999999999997229, 7.935100905948385908 ) ) ;
#10459 = CARTESIAN_POINT ( 'NONE',  ( -13.47710269719165588, 58.90286290043330553, -0.7859701997998082001 ) ) ;
#10460 = CARTESIAN_POINT ( 'NONE',  ( 10.42107401898988250, 45.10176735786057378, 8.582029462888934646 ) ) ;
#10461 = CARTESIAN_POINT ( 'NONE',  ( 11.99114687028902537, 69.65883756502691426, -6.201907584533547180 ) ) ;
#10462 = CARTESIAN_POINT ( 'NONE',  ( -8.343458848123582072, 67.37999999999998124, 11.48378591275253768 ) ) ;
#10463 = CARTESIAN_POINT ( 'NONE',  ( 12.17494424314613255, 30.21560166499141431, 5.835599225542421387 ) ) ;
#10464 = CARTESIAN_POINT ( 'NONE',  ( -8.113100482602192187, 55.48749888713909684, -10.81048510016282371 ) ) ;
#10465 = CARTESIAN_POINT ( 'NONE',  ( -8.613601466380250926, 50.34913078849175605, 10.39500302588977476 ) ) ;
#10466 = CARTESIAN_POINT ( 'NONE',  ( 7.870204901766977734, 63.88288127658925220, -10.96870105014976637 ) ) ;
#10467 = CARTESIAN_POINT ( 'NONE',  ( 7.482711392322309862, 42.89984591038155770, -11.23950954596197072 ) ) ;
#10468 = CARTESIAN_POINT ( 'NONE',  ( 12.48936162389965254, 39.24350828422937099, 5.125161080676649661 ) ) ;
#10469 = VERTEX_POINT ( 'NONE', #17032 ) ;
#10470 = CARTESIAN_POINT ( 'NONE',  ( -12.76659169606017841, 70.77175795909352018, -4.389135967592094012 ) ) ;
#10471 = CARTESIAN_POINT ( 'NONE',  ( -7.531934336383805828, 61.46230439911880694, -11.20387762871766313 ) ) ;
#10472 = VERTEX_POINT ( 'NONE', #3346 ) ;
#10473 = EDGE_CURVE ( 'NONE', #6360, #2328, #9010, .T. ) ;
#10474 = AXIS2_PLACEMENT_3D ( 'NONE', #47, #16114, #5452 ) ;
#10475 = CARTESIAN_POINT ( 'NONE',  ( -6.886120549656922663, 40.43470322261091354, -11.62389360686549722 ) ) ;
#10476 = ORIENTED_EDGE ( 'NONE', *, *, #10755, .T. ) ;
#10477 = CARTESIAN_POINT ( 'NONE',  ( 13.50000000000000000, 27.43000000000001037, 1.734723475976807094E-15 ) ) ;
#10478 = CARTESIAN_POINT ( 'NONE',  ( 0.000000000000000000, 5.918584287042170544, 0.000000000000000000 ) ) ;
#10479 = DIRECTION ( 'NONE',  ( 0.000000000000000000, 0.000000000000000000, 1.000000000000000000 ) ) ;
#10480 = CARTESIAN_POINT ( 'NONE',  ( 12.46436792225129508, 57.24116669652607214, 5.185512586538920665 ) ) ;
#10481 = CARTESIAN_POINT ( 'NONE',  ( 3.636496289402157078, 77.03000000000000114, -11.19198476289190936 ) ) ;
#10482 = CARTESIAN_POINT ( 'NONE',  ( 2.272985001014427788E-15, 80.18000000000000682, -12.37355403259654985 ) ) ;
#10483 = CARTESIAN_POINT ( 'NONE',  ( -0.1736399972044732620, 47.67375642894414511, 13.49917766817768339 ) ) ;
#10484 = CARTESIAN_POINT ( 'NONE',  ( 11.38173386846534108, -99.99999999999998579, 0.8785756797233987836 ) ) ;
#10485 = DIRECTION ( 'NONE',  ( 0.000000000000000000, -1.000000000000000000, 0.000000000000000000 ) ) ;
#10486 = CARTESIAN_POINT ( 'NONE',  ( 11.37500000000000000, 4.439344646909156023E-16, 9.531744055041752924E-13 ) ) ;
#10487 = CYLINDRICAL_SURFACE ( 'NONE', #11207, 8.999999999999998224 ) ;
#10488 = CARTESIAN_POINT ( 'NONE',  ( 19.29752010712851984, 0.000000000000000000, -17.42428528562851042 ) ) ;
#10489 = CARTESIAN_POINT ( 'NONE',  ( -2.464184276881911995, 73.26860352173120816, -13.27409137780385429 ) ) ;
#10490 = VERTEX_POINT ( 'NONE', #944 ) ;
#10491 = VERTEX_POINT ( 'NONE', #9104 ) ;
#10492 = DIRECTION ( 'NONE',  ( 1.000000000000000000, 1.301042606982605567E-16, 0.000000000000000000 ) ) ;
#10493 = ORIENTED_EDGE ( 'NONE', *, *, #8281, .F. ) ;
#10494 = CARTESIAN_POINT ( 'NONE',  ( 2.621994543952811015E-15, 16.18000000000000327, -14.19474002721660355 ) ) ;
#10495 = CARTESIAN_POINT ( 'NONE',  ( 11.37499999999960210, -106.1093749999997584, 4.711679271994916540 ) ) ;
#10496 = CARTESIAN_POINT ( 'NONE',  ( -7.237748362078336939, 44.41032146096258515, 11.39663970212459176 ) ) ;
#10497 = CYLINDRICAL_SURFACE ( 'NONE', #11881, 1.999999999999997335 ) ;
#10498 = CARTESIAN_POINT ( 'NONE',  ( 11.32884907035391464, 66.70497250890650776, -7.345399851619622389 ) ) ;
#10499 = CARTESIAN_POINT ( 'NONE',  ( 4.171729424061789260, 50.82999999999999829, 12.83926296998457417 ) ) ;
#10500 = CARTESIAN_POINT ( 'NONE',  ( -4.802988300473575833, 71.50697978349295170, 12.61891950573222765 ) ) ;
#10501 =( REPRESENTATION_RELATIONSHIP ('NONE','NONE', #7275, #8052 ) REPRESENTATION_RELATIONSHIP_WITH_TRANSFORMATION ( #7695 )SHAPE_REPRESENTATION_RELATIONSHIP( ) );
#10502 = CARTESIAN_POINT ( 'NONE',  ( -18.62500000000064659, -75.96562499999980389, 7.714727599197335195 ) ) ;
#10503 = EDGE_CURVE ( 'NONE', #9086, #12936, #14685, .T. ) ;
#10504 = CARTESIAN_POINT ( 'NONE',  ( -13.38959891692747917, 67.86975879323100003, -1.725407304280444754 ) ) ;
#10505 = CARTESIAN_POINT ( 'NONE',  ( 13.16986379960055409, 5.168750000000006395, -13.16986379959834430 ) ) ;
#10506 = CIRCLE ( 'NONE', #4583, 12.00000000000000178 ) ;
#10507 = CARTESIAN_POINT ( 'NONE',  ( 6.335111093105661340, 54.94766729977810371, -11.92126117983150912 ) ) ;
#10508 = CARTESIAN_POINT ( 'NONE',  ( -13.16986379960055231, -27.05624999999993463, 13.16986379959834252 ) ) ;
#10509 = CARTESIAN_POINT ( 'NONE',  ( -11.50534062751997411, 65.19367442093394516, 7.062375311795522137 ) ) ;
#10510 = CARTESIAN_POINT ( 'NONE',  ( -2.138189944381199137, 43.60311857767973720, 13.50000000000001421 ) ) ;
#10511 = CARTESIAN_POINT ( 'NONE',  ( -11.27144135186879659, 35.20884229997658110, 7.430021984585419403 ) ) ;
#10512 = ORIENTED_EDGE ( 'NONE', *, *, #6120, .T. ) ;
#10513 = CARTESIAN_POINT ( 'NONE',  ( -13.49999999999999822, 8.780000000000004690, -4.386415899144240349 ) ) ;
#10514 = CARTESIAN_POINT ( 'NONE',  ( -11.32176554887916886, 32.20565710450659225, 7.353236199019049124 ) ) ;
#10515 = DIRECTION ( 'NONE',  ( -0.000000000000000000, 1.000000000000000000, -0.000000000000000000 ) ) ;
#10516 = CARTESIAN_POINT ( 'NONE',  ( 8.343458848123583849, -4.120000000000001883, -11.48378591275253768 ) ) ;
#10517 = CARTESIAN_POINT ( 'NONE',  ( -9.441479826001016207, 53.30963963675974071, 9.659188822020484011 ) ) ;
#10518 = CIRCLE ( 'NONE', #12498, 12.00000000000000178 ) ;
#10519 = CARTESIAN_POINT ( 'NONE',  ( 7.272992578804311492, 58.88000000000000256, -10.01041549318726709 ) ) ;
#10520 = CARTESIAN_POINT ( 'NONE',  ( -8.343458848123576743, 72.48000000000000398, -11.48378591275254301 ) ) ;
#10521 = CARTESIAN_POINT ( 'NONE',  ( 12.58419665743400628, 51.25262647264697335, 4.889168462974375906 ) ) ;
#10522 = CARTESIAN_POINT ( 'NONE',  ( -9.357762247734804362, 38.31343841487202440, 9.730492229755752120 ) ) ;
#10523 = CARTESIAN_POINT ( 'NONE',  ( 13.49767104495738401, 36.43897965465946953, -0.2631044504109197324 ) ) ;
#10524 = CARTESIAN_POINT ( 'NONE',  ( 8.043339635996298753, -55.11874999999988489, 8.043339635997652337 ) ) ;
#10525 = DIRECTION ( 'NONE',  ( 0.000000000000000000, 0.000000000000000000, -1.000000000000000000 ) ) ;
#10526 = CARTESIAN_POINT ( 'NONE',  ( -12.28277907283284698, 77.13527343425541005, 5.607119744471182443 ) ) ;
#10527 = VECTOR ( 'NONE', #12908, 1000.000000000000000 ) ;
#10528 = CARTESIAN_POINT ( 'NONE',  ( -11.05895565395609026, 80.22189889663263784, 7.743948080728770833 ) ) ;
#10529 = CARTESIAN_POINT ( 'NONE',  ( 11.76794919243112680, 11.58000000000000362, -3.823638476888993942 ) ) ;
#10530 = DIRECTION ( 'NONE',  ( -0.000000000000000000, -0.000000000000000000, 1.000000000000000000 ) ) ;
#10531 = ORIENTED_EDGE ( 'NONE', *, *, #277, .T. ) ;
#10532 = CARTESIAN_POINT ( 'NONE',  ( 7.272992578804308828, 7.980000000000000426, 10.01041549318726709 ) ) ;
#10533 = ORIENTED_EDGE ( 'NONE', *, *, #4247, .F. ) ;
#10534 = CARTESIAN_POINT ( 'NONE',  ( -3.636496289402155746, 54.52999999999999403, 11.19198476289190936 ) ) ;
#10535 = CARTESIAN_POINT ( 'NONE',  ( 11.37500000000039613, -77.04062499999979252, -4.711679271993004292 ) ) ;
#10536 = FACE_BOUND ( 'NONE', #4260, .T. ) ;
#10537 = CARTESIAN_POINT ( 'NONE',  ( -13.49999999999999822, -6.920000000000000817, 4.386415899144235908 ) ) ;
#10538 = CARTESIAN_POINT ( 'NONE',  ( 11.90151132640803944, 75.66574786089606164, -6.376363749881278409 ) ) ;
#10539 = CARTESIAN_POINT ( 'NONE',  ( 18.62499999999934985, -98.85937499999975842, 7.714727599200467800 ) ) ;
#10540 = CARTESIAN_POINT ( 'NONE',  ( -13.49999999999999822, 77.07999999999998408, 4.386415899144235908 ) ) ;
#10541 = CARTESIAN_POINT ( 'NONE',  ( 2.272985001014427788E-15, 41.17999999999999972, -12.37355403259654985 ) ) ;
#10542 = FACE_OUTER_BOUND ( 'NONE', #11446, .T. ) ;
#10543 = AXIS2_PLACEMENT_3D ( 'NONE', #15064, #9808, #13661 ) ;
#10544 = CARTESIAN_POINT ( 'NONE',  ( -13.46788654291206733, 58.89779059911582237, -0.9332917827898941088 ) ) ;
#10545 = EDGE_CURVE ( 'NONE', #16090, #5515, #15528, .T. ) ;
#10546 = CARTESIAN_POINT ( 'NONE',  ( 8.093304213249069790, 44.98702088532150611, 10.81425868566774895 ) ) ;
#10547 = CARTESIAN_POINT ( 'NONE',  ( 13.41529543626620757, 69.37743073738961641, 1.509923354937637852 ) ) ;
#10548 = B_SPLINE_CURVE_WITH_KNOTS ( 'NONE', 3,
 ( #10315, #7576, #6248, #14180 ),
 .UNSPECIFIED., .F., .F.,
 ( 4, 4 ),
 ( 0.5895808622224875117, 0.5895837205860048336 ),
 .UNSPECIFIED. ) ;
#10549 = CARTESIAN_POINT ( 'NONE',  ( -13.49999999999999822, 66.78000000000000114, -4.386415899144240349 ) ) ;
#10550 = CARTESIAN_POINT ( 'NONE',  ( 12.50000000000000000, -18.00000000000000355, -2.204364238465235822E-15 ) ) ;
#10551 = CARTESIAN_POINT ( 'NONE',  ( -2.436326588224761114, 55.26753496234241680, -13.28513367767414977 ) ) ;
#10552 = CARTESIAN_POINT ( 'NONE',  ( -10.73222887417678351, 50.24104608057613319, 8.192202916843667637 ) ) ;
#10553 = CARTESIAN_POINT ( 'NONE',  ( 7.611112758387253763, 63.89427894107092953, -11.15141948763443835 ) ) ;
#10554 = CARTESIAN_POINT ( 'NONE',  ( 11.14349067449326292, 42.71675866716687864, -7.620623970109671852 ) ) ;
#10555 = CARTESIAN_POINT ( 'NONE',  ( 13.34721606699788232, 39.35891505498212695, 2.027891307246981079 ) ) ;
#10556 = ORIENTED_EDGE ( 'NONE', *, *, #558, .F. ) ;
#10557 = CARTESIAN_POINT ( 'NONE',  ( -9.314018664953470861, 70.54409196600954601, -9.787303825282853253 ) ) ;
#10558 = CARTESIAN_POINT ( 'NONE',  ( -4.673977061459858362, 61.34833404053931361, -12.66657423768662305 ) ) ;
#10559 = CARTESIAN_POINT ( 'NONE',  ( 3.636496289402154414, 7.830000000000003624, 11.19198476289190758 ) ) ;
#10560 = ORIENTED_EDGE ( 'NONE', *, *, #2507, .F. ) ;
#10561 = ORIENTED_EDGE ( 'NONE', *, *, #7493, .T. ) ;
#10562 = CARTESIAN_POINT ( 'NONE',  ( 8.343458848123578520, 20.98000000000001464, 11.48378591275254124 ) ) ;
#10563 = CARTESIAN_POINT ( 'NONE',  ( 18.62500000000000000, -49.94999999999988205, 1.560692158462880521E-12 ) ) ;
#10564 = CARTESIAN_POINT ( 'NONE',  ( 5.028978472489433749, 47.86150763825980903, 12.52835470249129735 ) ) ;
#10565 = CARTESIAN_POINT ( 'NONE',  ( 13.37958125658008868, 57.49285659070703502, -1.800066904135027013 ) ) ;
#10566 = CARTESIAN_POINT ( 'NONE',  ( 7.272992578804308828, 69.97999999999998977, 10.01041549318726709 ) ) ;
#10567 = CARTESIAN_POINT ( 'NONE',  ( -7.272992578804307939, 80.48000000000000398, -10.01041549318726886 ) ) ;
#10568 = CARTESIAN_POINT ( 'NONE',  ( -0.2850622938858722311, 47.66975023300910408, 13.49700841942235918 ) ) ;
#10569 = EDGE_CURVE ( 'NONE', #14419, #13897, #14918, .T. ) ;
#10570 = CARTESIAN_POINT ( 'NONE',  ( 4.269545073161230775, -100.0000000000000284, 13.16816258391341421 ) ) ;
#10571 = CARTESIAN_POINT ( 'NONE',  ( -13.49999999999999822, 33.77999999999999403, -4.386415899144240349 ) ) ;
#10572 = CARTESIAN_POINT ( 'NONE',  ( -9.552639591052204498E-13, -29.13749999999993179, 11.37500000000000000 ) ) ;
#10573 = DIRECTION ( 'NONE',  ( -0.000000000000000000, -0.000000000000000000, 1.000000000000000000 ) ) ;
#10574 = CARTESIAN_POINT ( 'NONE',  ( 8.419288814318939274, 33.85814146373429878, -10.55389719033477292 ) ) ;
#10575 = CARTESIAN_POINT ( 'NONE',  ( -2.271044718833372222, 73.26165834582242553, -13.30761088842764295 ) ) ;
#10576 = ORIENTED_EDGE ( 'NONE', *, *, #3206, .F. ) ;
#10577 = ORIENTED_EDGE ( 'NONE', *, *, #2407, .T. ) ;
#10578 = CARTESIAN_POINT ( 'NONE',  ( 3.636496289402154414, 78.82999999999999829, 11.19198476289190936 ) ) ;
#10579 = ORIENTED_EDGE ( 'NONE', *, *, #206, .T. ) ;
#10580 = CARTESIAN_POINT ( 'NONE',  ( -7.714727599197334307, -12.45312499999998757, -18.62500000000064659 ) ) ;
#10581 = CARTESIAN_POINT ( 'NONE',  ( -6.789762389132963705, 44.42913898759260860, 11.67122559010108418 ) ) ;
#10582 = CARTESIAN_POINT ( 'NONE',  ( 8.847408738254074478, 8.062211465790062093, 15.67642540545352148 ) ) ;
#10583 = CARTESIAN_POINT ( 'NONE',  ( 11.87809514247365072, 66.66774229667706209, -6.421792920400507754 ) ) ;
#10584 = CARTESIAN_POINT ( 'NONE',  ( -10.92172942406178926, 46.62999999999999545, -7.935100905948389460 ) ) ;
#10585 = CARTESIAN_POINT ( 'NONE',  ( -3.171773181161692268, 71.56595516633068144, 13.12211643693878216 ) ) ;
#10586 = CIRCLE ( 'NONE', #3513, 1.999999999999998224 ) ;
#10587 = EDGE_CURVE ( 'NONE', #1796, #7861, #10922, .T. ) ;
#10588 = CARTESIAN_POINT ( 'NONE',  ( -1.564113515457998572E-12, -79.08749999999980673, 18.62500000000000000 ) ) ;
#10589 = CARTESIAN_POINT ( 'NONE',  ( -13.43350214447777979, 67.88349517729756144, -1.338323814899765818 ) ) ;
#10590 = CARTESIAN_POINT ( 'NONE',  ( -13.16986379960055409, -19.80624999999993463, 13.16986379959834252 ) ) ;
#10591 = CARTESIAN_POINT ( 'NONE',  ( 6.127710875979031080, 54.95599452305749821, -12.02960116012748948 ) ) ;
#10592 = CARTESIAN_POINT ( 'NONE',  ( 7.272992578804311492, 17.87999999999999190, -10.01041549318726709 ) ) ;
#10593 = DIRECTION ( 'NONE',  ( -0.000000000000000000, -1.000000000000000000, -0.000000000000000000 ) ) ;
#10594 = CARTESIAN_POINT ( 'NONE',  ( -12.55657707847996107, 65.11044514684080298, 4.970209462128218902 ) ) ;
#10595 = CARTESIAN_POINT ( 'NONE',  ( -7.264233121273926841, 35.40920166682224135, 11.37991948868003611 ) ) ;
#10596 = CARTESIAN_POINT ( 'NONE',  ( -4.171729424061791036, 18.53000000000001890, 12.83926296998457239 ) ) ;
#10597 = ORIENTED_EDGE ( 'NONE', *, *, #3724, .F. ) ;
#10598 = CARTESIAN_POINT ( 'NONE',  ( 2.445080149700053643E-15, 51.18000000000000682, -13.50000000000000000 ) ) ;
#10599 = CARTESIAN_POINT ( 'NONE',  ( -7.272992578804310604, 28.38000000000000966, 10.01041549318726709 ) ) ;
#10600 = CARTESIAN_POINT ( 'NONE',  ( -4.763038992625359569, 31.35156427714300165, -12.63378481403946552 ) ) ;
#10601 = CARTESIAN_POINT ( 'NONE',  ( 1.959398577741635616, 73.10957903055695795, -13.36603894048193908 ) ) ;
#10602 = CARTESIAN_POINT ( 'NONE',  ( 13.03631756181396995, 60.30489250172575311, 3.507832160399530164 ) ) ;
#10603 = CARTESIAN_POINT ( 'NONE',  ( -10.95368854796565650, 53.22816082705852381, 7.891413927665784200 ) ) ;
#10604 = CARTESIAN_POINT ( 'NONE',  ( 7.272992578804311492, 61.87999999999999545, -10.01041549318726709 ) ) ;
#10605 = CARTESIAN_POINT ( 'NONE',  ( 6.428591458046670759, 50.91606176058002120, 11.87836298906071519 ) ) ;
#10606 = CARTESIAN_POINT ( 'NONE',  ( -13.00484043580565086, 37.80058143574180463, -3.623669304979980854 ) ) ;
#10607 = CARTESIAN_POINT ( 'NONE',  ( 9.206534659575176249, 36.03913477569856383, 9.873698037947086448 ) ) ;
#10608 = CARTESIAN_POINT ( 'NONE',  ( 7.714727599200456254, -43.67187499999991473, -18.62499999999935341 ) ) ;
#10609 = CARTESIAN_POINT ( 'NONE',  ( -5.229807916748995034, 74.49090577273676672, 12.44584714537170633 ) ) ;
#10610 = CARTESIAN_POINT ( 'NONE',  ( -9.476141181518151768, 76.55243570330306113, -9.615298271795859719 ) ) ;
#10611 = CARTESIAN_POINT ( 'NONE',  ( -12.63999744390774183, 80.10245305523378079, 4.762197372853401944 ) ) ;
#10612 = CARTESIAN_POINT ( 'NONE',  ( 11.76794919243112325, 11.27999999999999936, 3.823638476888996163 ) ) ;
#10613 = CARTESIAN_POINT ( 'NONE',  ( 7.500000000000000888, 102.9299999999999073, 9.367496997597653419 ) ) ;
#10614 = CARTESIAN_POINT ( 'NONE',  ( -10.92172942406179104, 8.230000000000014637, 7.935100905948385908 ) ) ;
#10615 = CARTESIAN_POINT ( 'NONE',  ( -3.636496289402156190, 4.530000000000006466, 11.19198476289190758 ) ) ;
#10616 = CARTESIAN_POINT ( 'NONE',  ( 7.272992578804311492, 52.87999999999998835, -10.01041549318726886 ) ) ;
#10617 = CARTESIAN_POINT ( 'NONE',  ( -4.711679271993003404, -64.55312499999983800, -11.37500000000039613 ) ) ;
#10618 = CARTESIAN_POINT ( 'NONE',  ( -13.16986379960055231, -10.40624999999997513, 13.16986379959834252 ) ) ;
#10619 = CARTESIAN_POINT ( 'NONE',  ( -10.92172942406179104, -9.769999999999994245, 7.935100905948385908 ) ) ;
#10620 = LINE ( 'NONE', #12199, #8859 ) ;
#10621 = CARTESIAN_POINT ( 'NONE',  ( 3.667885382569292307, 76.04811590521021003, -12.99217945106073735 ) ) ;
#10622 = EDGE_CURVE ( 'NONE', #6499, #13554, #9598, .T. ) ;
#10623 = CARTESIAN_POINT ( 'NONE',  ( 4.171729424061791924, 69.03000000000000114, -12.83926296998457239 ) ) ;
#10624 = CARTESIAN_POINT ( 'NONE',  ( -3.636496289402155746, 42.53000000000000114, 11.19198476289190936 ) ) ;
#10625 = CARTESIAN_POINT ( 'NONE',  ( -11.96482485551292285, 58.69645965844525648, -6.333484686160312904 ) ) ;
#10626 =( BOUNDED_CURVE ( )  B_SPLINE_CURVE ( 2, ( #12669, #3383, #561, #5968, #15472, #8795, #16724, #4631, #14153, #9231, #5156, #7722, #3727 ),
 .UNSPECIFIED., .F., .T. ) 
 B_SPLINE_CURVE_WITH_KNOTS ( ( 3, 2, 2, 2, 2, 2, 3 ),
 ( 0.05470091489015040803, 0.05845616897609282742, 0.06596667714797772863, 0.07347718531986256740, 0.08098769349174740617, 0.08849820166363223106, 0.09225345574959326056 ),
 .UNSPECIFIED. ) 
 CURVE ( )  GEOMETRIC_REPRESENTATION_ITEM ( )  RATIONAL_B_SPLINE_CURVE ( ( 0.9755282581475767101, 0.9755282581475767101, 1.000000000000000000, 0.9510565162951534202, 1.000000000000000000, 0.9510565162951534202, 1.000000000000000000, 0.9510565162951534202, 1.000000000000000000, 0.9510565162951534202, 1.000000000000000000, 0.9755282581474559178, 0.9755282581475767101 ) ) 
 REPRESENTATION_ITEM ( '' )  );
#10627 = CARTESIAN_POINT ( 'NONE',  ( 2.919893365847839650, 44.78498848662554366, 13.18044854437260405 ) ) ;
#10628 = CARTESIAN_POINT ( 'NONE',  ( 12.01162584235229680, 69.65724634270705451, -6.162282692494446046 ) ) ;
#10629 = CARTESIAN_POINT ( 'NONE',  ( 2.138189944381238661, 58.75688142232026223, 13.50000000000000000 ) ) ;
#10630 = CARTESIAN_POINT ( 'NONE',  ( 10.95321195831160743, 30.13180978604457039, 7.892151158665086541 ) ) ;
#10631 = CARTESIAN_POINT ( 'NONE',  ( -10.15369422253785814, 55.58731133826776016, -8.896836259020886928 ) ) ;
#10632 = CARTESIAN_POINT ( 'NONE',  ( -5.368619122948546263, 50.48560663089287459, 12.38686502221418984 ) ) ;
#10633 = CARTESIAN_POINT ( 'NONE',  ( 13.47553014558564222, 63.40190322894259367, 0.8129172673421702910 ) ) ;
#10634 = CARTESIAN_POINT ( 'NONE',  ( 13.01146853698397088, 42.55849631815364376, -3.598855205904288201 ) ) ;
#10635 = CARTESIAN_POINT ( 'NONE',  ( 13.50321739804985732, 39.42843470989561894, 0.04034527670750228528 ) ) ;
#10636 = ORIENTED_EDGE ( 'NONE', *, *, #4932, .F. ) ;
#10637 = CARTESIAN_POINT ( 'NONE',  ( -4.853172931527291567, 70.35493761421939496, -12.59957856612076021 ) ) ;
#10638 = CARTESIAN_POINT ( 'NONE',  ( -1.376924736209377498, 61.22942669131018079, -13.43187964474915930 ) ) ;
#10639 = AXIS2_PLACEMENT_3D ( 'NONE', #3066, #16681, #430 ) ;
#10640 = CARTESIAN_POINT ( 'NONE',  ( -7.409984580736203970E-16, 7.679999999999995275, 12.37355403259654985 ) ) ;
#10641 = ORIENTED_EDGE ( 'NONE', *, *, #2092, .T. ) ;
#10642 = ORIENTED_EDGE ( 'NONE', *, *, #558, .T. ) ;
#10643 = CARTESIAN_POINT ( 'NONE',  ( 13.50000000000000355, 27.58000000000000895, -4.386415899144233244 ) ) ;
#10644 = CARTESIAN_POINT ( 'NONE',  ( -18.62500000000000000, -58.27499999999986358, -1.562973063126292555E-12 ) ) ;
#10645 = EDGE_CURVE ( 'NONE', #11531, #668, #14012, .T. ) ;
#10646 = CARTESIAN_POINT ( 'NONE',  ( 6.624002440913375978, 47.92407202630063523, 11.76319263586970010 ) ) ;
#10647 = CARTESIAN_POINT ( 'NONE',  ( -4.171729424061791036, 9.530000000000010019, 12.83926296998457239 ) ) ;
#10648 = CARTESIAN_POINT ( 'NONE',  ( 9.880830748590257784, 72.07300539084614854, 9.199255159373397106 ) ) ;
#10649 = CARTESIAN_POINT ( 'NONE',  ( 13.49993779747335942, 57.43171647853688455, -0.05021896834556438538 ) ) ;
#10650 = CARTESIAN_POINT ( 'NONE',  ( -11.76794919243112325, 69.08000000000001251, 3.823638476888994386 ) ) ;
#10651 = CARTESIAN_POINT ( 'NONE',  ( 9.520470885617717371, 73.73000000000000398, -6.917026985038131848 ) ) ;
#10652 = CARTESIAN_POINT ( 'NONE',  ( -11.36497532230790064, 47.20289303351260912, 7.286111716941032768 ) ) ;
#10653 = DIRECTION ( 'NONE',  ( -0.000000000000000000, 1.000000000000000000, -0.000000000000000000 ) ) ;
#10654 = CARTESIAN_POINT ( 'NONE',  ( 15.00421320149717097, -100.0000000000000000, 10.33632056195987481 ) ) ;
#10655 = CARTESIAN_POINT ( 'NONE',  ( -2.138189944381236884, 75.25688142232026223, -13.50000000000000000 ) ) ;
#10656 = CARTESIAN_POINT ( 'NONE',  ( -8.043339635997654113, -27.05624999999993463, 8.043339635996302306 ) ) ;
#10657 = DIRECTION ( 'NONE',  ( 0.000000000000000000, 1.000000000000000000, 0.000000000000000000 ) ) ;
#10658 = CARTESIAN_POINT ( 'NONE',  ( 11.99908723489971329, 33.65823093649722608, -6.186429237525048030 ) ) ;
#10659 = CARTESIAN_POINT ( 'NONE',  ( -9.649170248876741240, 73.56114326775332302, -9.441584397305010867 ) ) ;
#10660 = ORIENTED_EDGE ( 'NONE', *, *, #6794, .F. ) ;
#10661 = ORIENTED_EDGE ( 'NONE', *, *, #10904, .T. ) ;
#10662 = CARTESIAN_POINT ( 'NONE',  ( -7.272992578804307939, 74.47999999999998977, -10.01041549318727064 ) ) ;
#10663 = VERTEX_POINT ( 'NONE', #6772 ) ;
#10664 = CARTESIAN_POINT ( 'NONE',  ( -9.552639591052204498E-13, -53.03749999999988773, 11.37499999999999645 ) ) ;
#10665 = CARTESIAN_POINT ( 'NONE',  ( -10.15272881233574331, 44.27273562141181174, 8.897895435131198738 ) ) ;
#10666 = EDGE_CURVE ( 'NONE', #13385, #1377, #13011, .T. ) ;
#10667 = CARTESIAN_POINT ( 'NONE',  ( -7.499999999999997335, -24.01085892585522075, 8.949127168380917041 ) ) ;
#10668 = CARTESIAN_POINT ( 'NONE',  ( -8.343458848123582072, 47.37999999999998835, 11.48378591275254124 ) ) ;
#10669 = CARTESIAN_POINT ( 'NONE',  ( -5.685284667237421985, 71.47340530370703959, 12.24467241409343110 ) ) ;
#10670 = CARTESIAN_POINT ( 'NONE',  ( -7.714727599197334307, -47.90312499999986784, -18.62500000000064659 ) ) ;
#10671 = CARTESIAN_POINT ( 'NONE',  ( -12.81927299732829795, 68.08231120825506366, 4.232820650394039319 ) ) ;
#10672 = CARTESIAN_POINT ( 'NONE',  ( 13.16986379960055409, -11.48124999999995488, -13.16986379959834430 ) ) ;
#10673 = CARTESIAN_POINT ( 'NONE',  ( 10.54836534261182912, 54.75121614555988714, -8.425092043074821291 ) ) ;
#10674 = CARTESIAN_POINT ( 'NONE',  ( -3.636496289402152637, 18.33000000000001251, -11.19198476289190936 ) ) ;
#10675 = CARTESIAN_POINT ( 'NONE',  ( 7.714727599197338748, -80.12812499999981242, 18.62500000000063949 ) ) ;
#10676 = CARTESIAN_POINT ( 'NONE',  ( -13.45796656469188335, 64.89315254009517275, -1.064987061088984222 ) ) ;
#10677 = CARTESIAN_POINT ( 'NONE',  ( -9.611889644271915500, 35.30078168614076617, 9.481849804571114149 ) ) ;
#10678 = VERTEX_POINT ( 'NONE', #285 ) ;
#10679 = CARTESIAN_POINT ( 'NONE',  ( 10.92172942406178926, 50.13000000000000256, 7.935100905948387684 ) ) ;
#10680 = EDGE_CURVE ( 'NONE', #908, #8520, #8258, .T. ) ;
#10681 = CARTESIAN_POINT ( 'NONE',  ( -10.71852365211889335, 31.61759523208409917, -8.219185043125531109 ) ) ;
#10682 = CARTESIAN_POINT ( 'NONE',  ( 10.99999999999990941, 7.773118517290098062, 15.58845726811995824 ) ) ;
#10683 = CARTESIAN_POINT ( 'NONE',  ( 3.636496289402154414, -7.169999999999995488, 11.19198476289190758 ) ) ;
#10684 = CARTESIAN_POINT ( 'NONE',  ( 3.225602179493814781, 59.79598290809182259, 13.10898689560911379 ) ) ;
#10685 = CARTESIAN_POINT ( 'NONE',  ( 13.50000000000000355, -4.420000000000007923, -4.386415899144233244 ) ) ;
#10686 = CARTESIAN_POINT ( 'NONE',  ( -11.12850500992075808, 53.21771862217647708, 7.643148398810014399 ) ) ;
#10687 = CARTESIAN_POINT ( 'NONE',  ( 7.272992578804308828, 48.97999999999999687, 10.01041549318726709 ) ) ;
#10688 = APPLICATION_PROTOCOL_DEFINITION ( 'draft international standard', 'automotive_design', 1998, #17138 ) ;
#10689 = CARTESIAN_POINT ( 'NONE',  ( 8.343458848123583849, 65.87999999999999545, -11.48378591275253768 ) ) ;
#10690 = CARTESIAN_POINT ( 'NONE',  ( 11.13837427305282191, 51.14299245685476336, 7.631533066694935030 ) ) ;
#10691 = AXIS2_PLACEMENT_3D ( 'NONE', #17295, #15786, #14370 ) ;
#10692 = CARTESIAN_POINT ( 'NONE',  ( -8.103196614201737091, 37.48751268113657176, -10.79762506269431199 ) ) ;
#10693 = CARTESIAN_POINT ( 'NONE',  ( 11.16073815863965812, 36.14426946062943813, 7.595459063093625396 ) ) ;
#10694 = CARTESIAN_POINT ( 'NONE',  ( -7.714727599200466912, -18.69687499999997726, 18.62499999999935341 ) ) ;
#10695 = CARTESIAN_POINT ( 'NONE',  ( -0.6513326186324287503, 74.65658052450302762, 13.48429236608166448 ) ) ;
#10696 = CARTESIAN_POINT ( 'NONE',  ( -13.47320743554847589, 76.96033088227574126, 0.8785557905998884198 ) ) ;
#10697 = CARTESIAN_POINT ( 'NONE',  ( -9.234617383006181512, 80.31946446022799080, 9.849864266179150007 ) ) ;
#10698 = AXIS2_PLACEMENT_3D ( 'NONE', #932, #3499, #10237 ) ;
#10699 = CARTESIAN_POINT ( 'NONE',  ( 7.499999999999998224, 107.9394166107542787, 5.548846425319428732 ) ) ;
#10700 = CARTESIAN_POINT ( 'NONE',  ( -9.520470885617717371, 1.230000000000008864, 6.917026985038133624 ) ) ;
#10701 = CARTESIAN_POINT ( 'NONE',  ( -11.76794919243112325, 48.07999999999999119, 3.823638476888994830 ) ) ;
#10702 = CARTESIAN_POINT ( 'NONE',  ( 4.711679271993006957, -72.87812499999979821, 11.37500000000039613 ) ) ;
#10703 = CARTESIAN_POINT ( 'NONE',  ( -13.16986379959834252, -39.54374999999990337, -13.16986379960055054 ) ) ;
#10704 = CARTESIAN_POINT ( 'NONE',  ( 4.171729424061789260, -9.169999999999998153, 12.83926296998457239 ) ) ;
#10705 = CARTESIAN_POINT ( 'NONE',  ( 11.37637957285810586, -100.0000000000000000, 0.000000000000000000 ) ) ;
#10706 = CARTESIAN_POINT ( 'NONE',  ( 12.45777842108767608, 75.61978625587052250, -5.214092426080158660 ) ) ;
#10707 = AXIS2_PLACEMENT_3D ( 'NONE', #4910, #8902, #9166 ) ;
#10708 = CARTESIAN_POINT ( 'NONE',  ( -18.62500000000000000, -91.57499999999977547, -1.562973063126292555E-12 ) ) ;
#10709 = CARTESIAN_POINT ( 'NONE',  ( -9.520470885617715595, 38.62999999999999545, -6.917026985038136289 ) ) ;
#10710 = CARTESIAN_POINT ( 'NONE',  ( -7.774974083674261571, 41.38732224484842703, 11.04531834479223917 ) ) ;
#10711 = CARTESIAN_POINT ( 'NONE',  ( -9.145099759719814259, 58.53607511944338881, -9.932359848896243903 ) ) ;
#10712 = B_SPLINE_CURVE_WITH_KNOTS ( 'NONE', 3,
 ( #17062, #3376, #15724, #8788 ),
 .UNSPECIFIED., .F., .F.,
 ( 4, 4 ),
 ( 2.383248697944731098E-07, 0.007646667935218613710 ),
 .UNSPECIFIED. ) ;
#10713 = CARTESIAN_POINT ( 'NONE',  ( 6.296202951178191398, 44.91078442072279842, 11.94188463877171458 ) ) ;
#10714 = CARTESIAN_POINT ( 'NONE',  ( 0.000000000000000000, -1.200000000000000030E-05, 0.000000000000000000 ) ) ;
#10715 = EDGE_CURVE ( 'NONE', #7293, #13128, #2491, .T. ) ;
#10716 = CARTESIAN_POINT ( 'NONE',  ( -12.08201809334919830, 55.70826805169760831, -6.022897540302621699 ) ) ;
#10717 = CARTESIAN_POINT ( 'NONE',  ( -13.27145342533492212, 49.84287066452262849, -2.473646717969534503 ) ) ;
#10718 = CARTESIAN_POINT ( 'NONE',  ( 10.96675222851313514, 63.72739450245582304, -7.884886543510749135 ) ) ;
#10719 = CARTESIAN_POINT ( 'NONE',  ( 5.656850990071720986, 42.97450686619443871, -12.25765484162504215 ) ) ;
#10720 = CARTESIAN_POINT ( 'NONE',  ( 13.48307184846283491, 39.45330054262541353, -0.6758713956733961581 ) ) ;
#10721 = VERTEX_POINT ( 'NONE', #8168 ) ;
#10722 = CARTESIAN_POINT ( 'NONE',  ( -5.553750751693518062, 70.38149911725399477, -12.30503917794814939 ) ) ;
#10723 = CARTESIAN_POINT ( 'NONE',  ( -0.5774508230433464950, 61.20074394919704730, -13.49036888543782275 ) ) ;
#10724 = ORIENTED_EDGE ( 'NONE', *, *, #10904, .F. ) ;
#10725 = EDGE_LOOP ( 'NONE', ( #16994, #5121, #13468, #2129 ) ) ;
#10726 = CARTESIAN_POINT ( 'NONE',  ( -8.343458848123582072, 26.37999999999999901, 11.48378591275254124 ) ) ;
#10727 = CARTESIAN_POINT ( 'NONE',  ( 13.16986379960055054, -52.03124999999987921, -13.16986379959834430 ) ) ;
#10728 = CARTESIAN_POINT ( 'NONE',  ( 4.789765888146141570, 61.00743788133880230, -12.62174563288985141 ) ) ;
#10729 = CARTESIAN_POINT ( 'NONE',  ( 13.49999999999999822, 10.28000000000000114, 4.386415899144237684 ) ) ;
#10730 = B_SPLINE_CURVE_WITH_KNOTS ( 'NONE', 3,
 ( #2961, #11381, #7227, #13744, #12613, #11117 ),
 .UNSPECIFIED., .F., .F.,
 ( 4, 2, 4 ),
 ( 2.344180274388505696E-07, 0.0005321324433834107633, 0.001064030468739382692 ),
 .UNSPECIFIED. ) ;
#10731 = PLANE ( 'NONE',  #12198 ) ;
#10732 = CARTESIAN_POINT ( 'NONE',  ( 11.56040206224664502, 57.68997124128148357, -6.971880404141066911 ) ) ;
#10733 = CARTESIAN_POINT ( 'NONE',  ( 7.272992578804311492, 64.87999999999999545, -10.01041549318726709 ) ) ;
#10734 = CARTESIAN_POINT ( 'NONE',  ( -11.76794919243112325, 72.07999999999999829, 3.823638476888994386 ) ) ;
#10735 = CARTESIAN_POINT ( 'NONE',  ( -6.839096004689836583, 47.42708027506941448, 11.64121267617738553 ) ) ;
#10736 = PRODUCT_DEFINITION_CONTEXT ( 'detailed design', #2336, 'design' ) ;
#10737 = CARTESIAN_POINT ( 'NONE',  ( -8.343458848123578520, 45.47999999999998977, -11.48378591275254124 ) ) ;
#10738 = CARTESIAN_POINT ( 'NONE',  ( 17.54501034274306193, -99.99999999999994316, 5.877963988053037880 ) ) ;
#10739 = CARTESIAN_POINT ( 'NONE',  ( 7.999999999999849010, 0.000000000000000000, 24.73863375370601148 ) ) ;
#10740 = CARTESIAN_POINT ( 'NONE',  ( 11.37500000000039435, -1.040624999999997025, -4.711679271993004292 ) ) ;
#10741 = CARTESIAN_POINT ( 'NONE',  ( -13.49999999999999822, 39.77999999999998693, -4.386415899144240349 ) ) ;
#10742 = CARTESIAN_POINT ( 'NONE',  ( 12.05830588875037712, 33.65359821999817314, -6.070472308088694646 ) ) ;
#10743 = CARTESIAN_POINT ( 'NONE',  ( -3.658860937772914212, 73.31156020023337305, -12.99472133403736152 ) ) ;
#10744 = ORIENTED_EDGE ( 'NONE', *, *, #3581, .F. ) ;
#10745 = VERTEX_POINT ( 'NONE', #4262 ) ;
#10746 = CARTESIAN_POINT ( 'NONE',  ( -9.520470885617717371, 78.23000000000000398, 6.917026985038133624 ) ) ;
#10747 = ORIENTED_EDGE ( 'NONE', *, *, #3261, .F. ) ;
#10748 = CARTESIAN_POINT ( 'NONE',  ( 1.561832610794586740E-12, -11.41249999999999254, -18.62500000000000000 ) ) ;
#10749 = CARTESIAN_POINT ( 'NONE',  ( -4.276945109164544512, 44.52621246546315348, 12.80489214357455197 ) ) ;
#10750 = CARTESIAN_POINT ( 'NONE',  ( 8.708180880075632402, 8.055324230341707192, 15.78346433836038898 ) ) ;
#10751 = CARTESIAN_POINT ( 'NONE',  ( -8.343458848123576743, 40.47999999999999687, -11.48378591275254301 ) ) ;
#10752 = CARTESIAN_POINT ( 'NONE',  ( -13.49952901374136083, 70.92525494836556277, -0.1387502169606815439 ) ) ;
#10753 = VECTOR ( 'NONE', #5854, 1000.000000000000000 ) ;
#10754 = CARTESIAN_POINT ( 'NONE',  ( -18.62499999999935341, -33.33437499999990195, -7.714727599200458030 ) ) ;
#10755 = EDGE_CURVE ( 'NONE', #7575, #1725, #17201, .T. ) ;
#10756 = CARTESIAN_POINT ( 'NONE',  ( -13.40586589714901322, 67.87439773989004266, -1.595217673327048447 ) ) ;
#10757 = CARTESIAN_POINT ( 'NONE',  ( -7.714727599197335195, -88.45312499999978684, -18.62500000000064304 ) ) ;
#10758 = EDGE_CURVE ( 'NONE', #9365, #4394, #1421, .T. ) ;
#10759 = CARTESIAN_POINT ( 'NONE',  ( 13.49702819973023615, 54.44026504364671126, -0.2991497332704560752 ) ) ;
#10760 = CARTESIAN_POINT ( 'NONE',  ( 7.714727599200458030, -86.37187499999978968, -18.62499999999934985 ) ) ;
#10761 = CARTESIAN_POINT ( 'NONE',  ( -12.92775954166086549, 64.79065094487656040, -3.889038681538313114 ) ) ;
#10762 = CARTESIAN_POINT ( 'NONE',  ( -12.94307868198818845, 34.79255189543185622, -3.838412397159299605 ) ) ;
#10763 = CARTESIAN_POINT ( 'NONE',  ( 13.50000000000000355, 22.58000000000000895, -4.386415899144233244 ) ) ;
#10764 = EDGE_LOOP ( 'NONE', ( #12869, #7577, #10253, #6955 ) ) ;
#10765 = CARTESIAN_POINT ( 'NONE',  ( 0.000000000000000000, 80.93000000000000682, 0.000000000000000000 ) ) ;
#10766 = CARTESIAN_POINT ( 'NONE',  ( -5.471302638117776063, 31.37832158213074862, -12.34159723640939887 ) ) ;
#10767 = CARTESIAN_POINT ( 'NONE',  ( 5.935702408891331494, 72.96359331791715874, -12.12507858477615308 ) ) ;
#10768 = DIRECTION ( 'NONE',  ( 1.000000000000000000, 8.673617379884035472E-17, 0.000000000000000000 ) ) ;
#10769 = CARTESIAN_POINT ( 'NONE',  ( 13.50000000000000355, -7.419999999999999929, -4.386415899144233244 ) ) ;
#10770 = CARTESIAN_POINT ( 'NONE',  ( -5.697279727035623687, 53.47290833051743419, 12.24689732723735425 ) ) ;
#10771 = CARTESIAN_POINT ( 'NONE',  ( -3.636496289402155746, 45.53000000000000114, 11.19198476289190936 ) ) ;
#10772 = APPLICATION_PROTOCOL_DEFINITION ( 'draft international standard', 'automotive_design', 1998, #4161 ) ;
#10773 = CARTESIAN_POINT ( 'NONE',  ( 10.92172942406178926, 71.12999999999999545, 7.935100905948387684 ) ) ;
#10774 = CARTESIAN_POINT ( 'NONE',  ( 5.061740244522564325, 50.86273991812466022, 12.51519464505669887 ) ) ;
#10775 = CARTESIAN_POINT ( 'NONE',  ( -13.21301978975160729, 37.83156230358514449, -2.785450445402589015 ) ) ;
#10776 = ADVANCED_FACE ( 'NONE', ( #13619, #14935 ), #12128, .T. ) ;
#10777 = CARTESIAN_POINT ( 'NONE',  ( 6.741550819447308385, 35.92884056994786590, 11.69833314936273894 ) ) ;
#10778 = CARTESIAN_POINT ( 'NONE',  ( -1.564113515457998370E-12, -36.38749999999993179, 18.62500000000000000 ) ) ;
#10779 = CARTESIAN_POINT ( 'NONE',  ( -11.99481679410065382, 74.15856145072713446, 6.194708363428219400 ) ) ;
#10780 = CARTESIAN_POINT ( 'NONE',  ( -10.55318980305114884, 76.60867959057283372, -8.423370909350431646 ) ) ;
#10781 = CARTESIAN_POINT ( 'NONE',  ( -11.69703628230260151, 79.67889527854070764, -6.754490024069266241 ) ) ;
#10782 = CARTESIAN_POINT ( 'NONE',  ( -7.272992578804310604, 10.37999999999999901, 10.01041549318726709 ) ) ;
#10783 = CARTESIAN_POINT ( 'NONE',  ( 1.668451422296014508, 80.93000000000003524, 13.07629037559565610 ) ) ;
#10784 = CARTESIAN_POINT ( 'NONE',  ( 11.76794919243112325, -0.7200000000000004174, 3.823638476888996163 ) ) ;
#10785 = CARTESIAN_POINT ( 'NONE',  ( 11.76794919243112325, 52.28000000000000114, 3.823638476888997051 ) ) ;
#10786 = CARTESIAN_POINT ( 'NONE',  ( 4.711679271994909435, -19.77187499999995168, -11.37499999999960387 ) ) ;
#10787 = CARTESIAN_POINT ( 'NONE',  ( 7.714727599197338748, -30.17812499999993747, 18.62500000000063949 ) ) ;
#10788 = CARTESIAN_POINT ( 'NONE',  ( 8.343458848123583849, -5.120000000000007212, -11.48378591275253768 ) ) ;
#10789 = CARTESIAN_POINT ( 'NONE',  ( -12.98636831301070060, 40.79815473098589962, -3.688632511342929465 ) ) ;
#10790 = CIRCLE ( 'NONE', #3164, 22.50000000000000355 ) ;
#10791 = DIRECTION ( 'NONE',  ( -0.8660254037844365982, -0.000000000000000000, -0.5000000000000036637 ) ) ;
#10792 = CARTESIAN_POINT ( 'NONE',  ( 11.33580039144190899, 75.15524277601195990, 7.331465318532246478 ) ) ;
#10793 = CARTESIAN_POINT ( 'NONE',  ( 13.50000000000000000, 32.42999999999999972, 1.653273178848926867E-15 ) ) ;
#10794 = CARTESIAN_POINT ( 'NONE',  ( 10.92172942406179104, 50.72999999999999687, -7.935100905948385908 ) ) ;
#10795 = CARTESIAN_POINT ( 'NONE',  ( 3.636496289402154414, 39.82999999999999829, 11.19198476289190936 ) ) ;
#10796 = CARTESIAN_POINT ( 'NONE',  ( -5.328320514085317150, 41.48727112542576378, 12.41054507597009149 ) ) ;
#10797 = CARTESIAN_POINT ( 'NONE',  ( -8.769463355901507384, 58.51817495466201535, -10.26385875965554462 ) ) ;
#10798 = CARTESIAN_POINT ( 'NONE',  ( -7.416407864998736166, 9.346025403784448571, -10.20780970022448031 ) ) ;
#10799 = AXIS2_PLACEMENT_3D ( 'NONE', #11629, #15408, #2231 ) ;
#10800 = EDGE_CURVE ( 'NONE', #2220, #11282, #16003, .T. ) ;
#10801 = CARTESIAN_POINT ( 'NONE',  ( 10.92172942406179104, 59.73000000000000398, -7.935100905948385908 ) ) ;
#10802 = CARTESIAN_POINT ( 'NONE',  ( -9.708203932499369415, 4.363974596215572710, 7.053423027509678533 ) ) ;
#10803 = CARTESIAN_POINT ( 'NONE',  ( -3.708203932499378297, 1.663974596215580748, 11.41267819554186858 ) ) ;
#10804 = CARTESIAN_POINT ( 'NONE',  ( -7.425691233511519940, 49.45773034968338777, -11.27429194107610044 ) ) ;
#10805 = CARTESIAN_POINT ( 'NONE',  ( 13.22478289187903222, 63.52662974475261137, -2.734757776350366321 ) ) ;
#10806 = CARTESIAN_POINT ( 'NONE',  ( 12.65298316251227284, 42.60172510704381210, -4.748097754914298640 ) ) ;
#10807 = CARTESIAN_POINT ( 'NONE',  ( -18.46851087777848477, 7.924527533097216470, 1.297848593170422893 ) ) ;
#10808 = VERTEX_POINT ( 'NONE', #5513 ) ;
#10809 = CARTESIAN_POINT ( 'NONE',  ( -4.711679271994915652, -11.44687499999997371, 11.37499999999960210 ) ) ;
#10810 = CARTESIAN_POINT ( 'NONE',  ( 13.49999999999999822, 12.28000000000001002, 4.386415899144237684 ) ) ;
#10811 = ORIENTED_EDGE ( 'NONE', *, *, #7215, .T. ) ;
#10812 = CARTESIAN_POINT ( 'NONE',  ( -7.347982688691526043, 43.45433612642857923, -11.33561514380692792 ) ) ;
#10813 = CARTESIAN_POINT ( 'NONE',  ( 1.561832610794586538E-12, -54.11249999999986926, -18.62500000000000000 ) ) ;
#10814 = CARTESIAN_POINT ( 'NONE',  ( 12.45342510802381497, 60.62052796052494585, -5.234417581101719286 ) ) ;
#10815 = CARTESIAN_POINT ( 'NONE',  ( 13.50000000000000000, 16.42999999999999972, 1.734723475976807094E-15 ) ) ;
#10816 = CIRCLE ( 'NONE', #15864, 6.000000000000000000 ) ;
#10817 = CARTESIAN_POINT ( 'NONE',  ( 9.768097186728329717, 72.06720429639440795, 9.318491340992334671 ) ) ;
#10818 = CARTESIAN_POINT ( 'NONE',  ( 13.47581130843072650, 57.39853584928295049, 0.9114065446593455633 ) ) ;
#10819 = CARTESIAN_POINT ( 'NONE',  ( -3.636496289402155746, 69.53000000000001535, 11.19198476289190936 ) ) ;
#10820 = CARTESIAN_POINT ( 'NONE',  ( 11.76794919243112680, 79.57999999999999829, -3.823638476888993942 ) ) ;
#10821 = CARTESIAN_POINT ( 'NONE',  ( -9.976789923895726275, 47.28199978130749059, 9.094920084438699703 ) ) ;
#10822 = DIRECTION ( 'NONE',  ( -0.000000000000000000, 1.000000000000000000, -0.000000000000000000 ) ) ;
#10823 = CARTESIAN_POINT ( 'NONE',  ( 4.171729424061789260, 73.83000000000001251, 12.83926296998457417 ) ) ;
#10824 = CARTESIAN_POINT ( 'NONE',  ( 8.343458848123580296, 37.97999999999999687, 11.48378591275253768 ) ) ;
#10825 = CARTESIAN_POINT ( 'NONE',  ( -2.138189944381230223, 76.60311857767973720, 13.50000000000000178 ) ) ;
#10826 = CARTESIAN_POINT ( 'NONE',  ( -8.043339635997654113, -86.40624999999977263, 8.043339635996304082 ) ) ;
#10827 = CARTESIAN_POINT ( 'NONE',  ( -2.138189944381240881, 40.60311857767972299, 13.49999999999999822 ) ) ;
#10828 = CARTESIAN_POINT ( 'NONE',  ( 13.37800033110732478, 33.36627688407902070, 1.820700357919406542 ) ) ;
#10829 = CARTESIAN_POINT ( 'NONE',  ( -5.415842637199018483, 73.37609553661370398, -12.37091407123440412 ) ) ;
#10830 = ORIENTED_EDGE ( 'NONE', *, *, #4834, .T. ) ;
#10831 = EDGE_LOOP ( 'NONE', ( #152, #6411, #12151, #14332 ) ) ;
#10832 = CARTESIAN_POINT ( 'NONE',  ( 11.76794919243112325, 23.43000000000000682, 1.734723475976807094E-15 ) ) ;
#10833 = CARTESIAN_POINT ( 'NONE',  ( -4.084710662422550875, 62.53312106380167990, 12.86754019334286703 ) ) ;
#10834 = ORIENTED_EDGE ( 'NONE', *, *, #13434, .F. ) ;
#10835 = CARTESIAN_POINT ( 'NONE',  ( 11.37500000000039613, -58.24062499999988063, -4.711679271993002516 ) ) ;
#10836 = CARTESIAN_POINT ( 'NONE',  ( -11.20293937805184470, 44.21312063056868880, 7.532871974709584251 ) ) ;
#10837 = CARTESIAN_POINT ( 'NONE',  ( -10.92172942406179104, 44.22999999999999687, 7.935100905948387684 ) ) ;
#10838 = CARTESIAN_POINT ( 'NONE',  ( 13.50000000000000355, 47.57999999999999119, -4.386415899144233244 ) ) ;
#10839 = CARTESIAN_POINT ( 'NONE',  ( -12.50265387745223222, 71.11554310126858525, 5.102506177351393113 ) ) ;
#10840 = CARTESIAN_POINT ( 'NONE',  ( -7.714727599200466912, -54.14687499999985931, 18.62499999999935341 ) ) ;
#10841 = CARTESIAN_POINT ( 'NONE',  ( -13.45717572954313646, 67.96817528193095370, 1.102425897065126392 ) ) ;
#10842 = CARTESIAN_POINT ( 'NONE',  ( 7.714727599197340524, -22.92812499999992326, 18.62500000000063949 ) ) ;
#10843 = CARTESIAN_POINT ( 'NONE',  ( 12.98222888748651727, 54.29759349226736731, 3.703881015682214617 ) ) ;
#10844 = CYLINDRICAL_SURFACE ( 'NONE', #6761, 26.00000000000000355 ) ;
#10845 = CARTESIAN_POINT ( 'NONE',  ( -11.88702157392819814, 64.69325053915714818, -6.399122214038043488 ) ) ;
#10846 = ORIENTED_EDGE ( 'NONE', *, *, #5899, .F. ) ;
#10847 = CARTESIAN_POINT ( 'NONE',  ( -13.35126160523930139, 34.99999482559385200, 1.998514373049085746 ) ) ;
#10848 = CARTESIAN_POINT ( 'NONE',  ( 13.50000000000000000, 22.43000000000000682, 1.734723475976807094E-15 ) ) ;
#10849 = ORIENTED_EDGE ( 'NONE', *, *, #5434, .F. ) ;
#10850 = CARTESIAN_POINT ( 'NONE',  ( 12.50000000000000000, -18.00000000000000355, -2.204364238465235822E-15 ) ) ;
#10851 = CARTESIAN_POINT ( 'NONE',  ( -4.344788714333951418, 31.33625517492832913, -12.78223156099206470 ) ) ;
#10852 = CARTESIAN_POINT ( 'NONE',  ( 4.710849725239000030, 73.01037628082356434, -12.65146089665251417 ) ) ;
#10853 = CARTESIAN_POINT ( 'NONE',  ( -1.545162525932825686E-06, 79.18000005555833809, -13.49999999999990941 ) ) ;
#10854 = EDGE_CURVE ( 'NONE', #2583, #7126, #16959, .T. ) ;
#10855 = CARTESIAN_POINT ( 'NONE',  ( 13.49999999999999822, -16.72000000000000597, 4.386415899144237684 ) ) ;
#10856 = CARTESIAN_POINT ( 'NONE',  ( -10.92172942406178926, 76.63000000000000966, -7.935100905948389460 ) ) ;
#10857 = CARTESIAN_POINT ( 'NONE',  ( -13.25030927750719023, 52.83740350991146784, -2.625255815485765254 ) ) ;
#10858 = CARTESIAN_POINT ( 'NONE',  ( -3.636496289402153081, 47.32999999999999829, -11.19198476289190936 ) ) ;
#10859 = CARTESIAN_POINT ( 'NONE',  ( -13.49999999999999822, 64.07999999999999829, 4.386415899144235908 ) ) ;
#10860 = CARTESIAN_POINT ( 'NONE',  ( 10.71528539912113587, 51.11814703885590916, 8.211795539909561015 ) ) ;
#10861 = CARTESIAN_POINT ( 'NONE',  ( -8.262753881998353478, 37.49471052164448537, -10.67663033658361194 ) ) ;
#10862 = CIRCLE ( 'NONE', #5516, 12.00000000000000178 ) ;
#10863 = CARTESIAN_POINT ( 'NONE',  ( 4.171617934058110322, 35.82999575861108355, 12.83930447791230733 ) ) ;
#10864 = CARTESIAN_POINT ( 'NONE',  ( 7.714727599200456254, -27.02187499999995524, -18.62499999999935341 ) ) ;
#10865 = CARTESIAN_POINT ( 'NONE',  ( -12.20819043409092686, 74.14144561344353690, 5.764729960070299697 ) ) ;
#10866 = CARTESIAN_POINT ( 'NONE',  ( -13.31362382857851401, 76.85144516294874961, -2.236570268612275481 ) ) ;
#10867 = CARTESIAN_POINT ( 'NONE',  ( -11.99286688454158423, 80.15883121440852221, 6.202559419596111567 ) ) ;
#10868 = CARTESIAN_POINT ( 'NONE',  ( 15.58845726811984811, 0.000000000000000000, 11.00000000000007283 ) ) ;
#10869 = DIRECTION ( 'NONE',  ( -0.000000000000000000, -1.000000000000000000, -0.000000000000000000 ) ) ;
#10870 = CARTESIAN_POINT ( 'NONE',  ( 0.000000000000000000, 108.9300000000000068, 0.000000000000000000 ) ) ;
#10871 = CARTESIAN_POINT ( 'NONE',  ( 9.520470885617715595, 2.129999999999992788, 6.917026985038135400 ) ) ;
#10872 = CARTESIAN_POINT ( 'NONE',  ( -7.272992578804310604, 48.38000000000000256, 10.01041549318726886 ) ) ;
#10873 = CARTESIAN_POINT ( 'NONE',  ( -4.711679271994916540, -11.44687499999997371, 11.37499999999960210 ) ) ;
#10874 = CARTESIAN_POINT ( 'NONE',  ( 13.16986379959834075, -14.56874999999996589, 13.16986379960055231 ) ) ;
#10875 = CARTESIAN_POINT ( 'NONE',  ( 2.621994543952811015E-15, -10.82000000000000206, -14.19474002721660355 ) ) ;
#10876 = CARTESIAN_POINT ( 'NONE',  ( -9.271068558427053574, 40.54190090920804579, -9.832000470486038424 ) ) ;
#10877 = CARTESIAN_POINT ( 'NONE',  ( -2.754321577462427229, 34.27903524419202341, -13.21604803840751075 ) ) ;
#10878 = CARTESIAN_POINT ( 'NONE',  ( 13.42050293043087628, 75.37783193970557249, 1.493644694584513877 ) ) ;
#10879 = EDGE_CURVE ( 'NONE', #16659, #11880, #4224, .T. ) ;
#10880 = CARTESIAN_POINT ( 'NONE',  ( 12.99792880889490121, -5.025561147605685224E-16, -12.49106143210709696 ) ) ;
#10881 =( BOUNDED_CURVE ( )  B_SPLINE_CURVE ( 2, ( #328, #5824, #1902, #16405, #4306, #11291, #9983, #9718, #9896, #15330, #3142, #1645, #1732 ),
 .UNSPECIFIED., .F., .F. ) 
 B_SPLINE_CURVE_WITH_KNOTS ( ( 3, 2, 2, 2, 2, 2, 3 ),
 ( 0.8750000000000000000, 0.8777777777777777679, 0.8833333333333333037, 0.8888888888888888395, 0.8944444444444444864, 0.9000000000000000222, 0.9027777777777777901 ),
 .UNSPECIFIED. ) 
 CURVE ( )  GEOMETRIC_REPRESENTATION_ITEM ( )  RATIONAL_B_SPLINE_CURVE ( ( 0.9755282581475768211, 0.9755282581475768211, 1.000000000000000000, 0.9510565162951535312, 1.000000000000000000, 0.9510565162951535312, 1.000000000000000000, 0.9510565162951535312, 1.000000000000000000, 0.9510565162951535312, 1.000000000000000000, 0.9755282581475768211, 0.9755282581475768211 ) ) 
 REPRESENTATION_ITEM ( '' )  );
#10882 = CARTESIAN_POINT ( 'NONE',  ( 3.636496289402157078, 32.02999999999999403, -11.19198476289190936 ) ) ;
#10883 = CARTESIAN_POINT ( 'NONE',  ( -9.328174606224918008, 41.31489523830415322, 9.758853723763433408 ) ) ;
#10884 = CARTESIAN_POINT ( 'NONE',  ( -5.766677717960000393, 58.38977191998154126, -12.20636860387775968 ) ) ;
#10885 = CIRCLE ( 'NONE', #8931, 9.000000000000000000 ) ;
#10886 = CARTESIAN_POINT ( 'NONE',  ( 4.819556118089159291, 44.85366279358599684, 12.61109904234389134 ) ) ;
#10887 = DIRECTION ( 'NONE',  ( -0.000000000000000000, -1.000000000000000000, -0.000000000000000000 ) ) ;
#10888 = CARTESIAN_POINT ( 'NONE',  ( 11.27030629789887151, 30.15099789552461118, 7.433993972937317452 ) ) ;
#10889 = CARTESIAN_POINT ( 'NONE',  ( 4.178864255851000829E-14, 61.67999999999999261, 13.50000000000000000 ) ) ;
#10890 = CARTESIAN_POINT ( 'NONE',  ( -11.11345371158683193, 49.64136890623429821, -7.664617922830998076 ) ) ;
#10891 = CARTESIAN_POINT ( 'NONE',  ( 13.43761406456407492, 63.38425578468477539, 1.321427766813064730 ) ) ;
#10892 = CARTESIAN_POINT ( 'NONE',  ( 12.41764327119240008, 42.23685895187078643, 5.297586243279120310 ) ) ;
#10893 = CARTESIAN_POINT ( 'NONE',  ( 1.767417051738310985, 49.11645020481132917, -13.49999950439118379 ) ) ;
#10894 = ORIENTED_EDGE ( 'NONE', *, *, #2855, .T. ) ;
#10895 = CARTESIAN_POINT ( 'NONE',  ( -3.095780066046758261, 70.29131268516505315, -13.14851532330129480 ) ) ;
#10896 = CARTESIAN_POINT ( 'NONE',  ( -2.138189944381240881, 49.60311857767973009, 13.49999999999999822 ) ) ;
#10897 = CARTESIAN_POINT ( 'NONE',  ( -4.171729424061791036, 11.53000000000001180, 12.83926296998457239 ) ) ;
#10898 = ORIENTED_EDGE ( 'NONE', *, *, #160, .T. ) ;
#10899 = CARTESIAN_POINT ( 'NONE',  ( -11.10089580902282158, 43.64063000482338595, -7.682467894417619902 ) ) ;
#10900 = CARTESIAN_POINT ( 'NONE',  ( -7.500000000000000000, 104.2024577724304208, -9.199283337799345261 ) ) ;
#10901 = CARTESIAN_POINT ( 'NONE',  ( 10.46746661683255653, 60.75568857945317092, -8.525446913291563789 ) ) ;
#10902 = AXIS2_PLACEMENT_3D ( 'NONE', #12998, #880, #15682 ) ;
#10903 = CARTESIAN_POINT ( 'NONE',  ( 13.50000000000000000, 13.42999999999999794, 1.734723475976807094E-15 ) ) ;
#10904 = EDGE_CURVE ( 'NONE', #1713, #14459, #17058, .T. ) ;
#10905 = CARTESIAN_POINT ( 'NONE',  ( -7.714727599200466912, -11.44687499999997371, 18.62499999999934985 ) ) ;
#10906 = CARTESIAN_POINT ( 'NONE',  ( 9.849129003214182276, 66.78863070281131797, -9.232880278536482521 ) ) ;
#10907 = CARTESIAN_POINT ( 'NONE',  ( 4.773345198892768870, 56.85194987062286032, 12.62857154888958888 ) ) ;
#10908 = CARTESIAN_POINT ( 'NONE',  ( 9.520470885617717371, 73.73000000000000398, -6.917026985038131848 ) ) ;
#10909 = CARTESIAN_POINT ( 'NONE',  ( 9.520470885617717371, 70.73000000000000398, -6.917026985038131848 ) ) ;
#10910 = CARTESIAN_POINT ( 'NONE',  ( -9.897695747161748159, 47.28611403347316866, 9.180720129038011379 ) ) ;
#10911 = DIRECTION ( 'NONE',  ( 0.000000000000000000, -1.000000000000000000, 0.000000000000000000 ) ) ;
#10912 = CARTESIAN_POINT ( 'NONE',  ( -7.779800476318354832E-16, 7.813974596215564006, 12.00000000000000355 ) ) ;
#10913 = CARTESIAN_POINT ( 'NONE',  ( 3.629376248049960729, -100.0000000000000711, 14.61214224149137841 ) ) ;
#10914 = CARTESIAN_POINT ( 'NONE',  ( -2.762017976112265849, 56.58058146214491302, 13.21593017864399933 ) ) ;
#10915 = CARTESIAN_POINT ( 'NONE',  ( 8.043339635996300530, -47.86874999999988489, 8.043339635997654113 ) ) ;
#10916 = AXIS2_PLACEMENT_3D ( 'NONE', #1012, #11978, #6681 ) ;
#10917 = DIRECTION ( 'NONE',  ( 0.000000000000000000, 0.000000000000000000, 1.000000000000000000 ) ) ;
#10918 = CARTESIAN_POINT ( 'NONE',  ( 13.22184478347566206, 33.52670040130352902, -2.737004561010502268 ) ) ;
#10919 = CARTESIAN_POINT ( 'NONE',  ( -8.000000000000197176, 0.000000000000000000, 24.73863375370590134 ) ) ;
#10920 = CARTESIAN_POINT ( 'NONE',  ( -9.870106908097179499, 8.002076557278329005, -15.32050807568887940 ) ) ;
#10921 = ORIENTED_EDGE ( 'NONE', *, *, #9277, .F. ) ;
#10922 = LINE ( 'NONE', #6953, #4211 ) ;
#10923 = ORIENTED_EDGE ( 'NONE', *, *, #7001, .T. ) ;
#10924 = CARTESIAN_POINT ( 'NONE',  ( -13.47797578622742698, 40.90339952845120308, -0.7708587157098785170 ) ) ;
#10925 = CARTESIAN_POINT ( 'NONE',  ( -9.520470885617715595, -14.37000000000000099, -6.917026985038136289 ) ) ;
#10926 = CARTESIAN_POINT ( 'NONE',  ( 13.16986379959833897, -21.81874999999996589, 13.16986379960055409 ) ) ;
#10927 = CARTESIAN_POINT ( 'NONE',  ( -13.32560535323595907, 44.00666090964475075, 2.189336705854063148 ) ) ;
#10928 = CARTESIAN_POINT ( 'NONE',  ( -10.85006967914022979, 7.815232006635826956, 15.50189495701166464 ) ) ;
#10929 = CIRCLE ( 'NONE', #13178, 13.50000000000000000 ) ;
#10930 = CARTESIAN_POINT ( 'NONE',  ( 4.171729424061789260, 47.82999999999999829, 12.83926296998457417 ) ) ;
#10931 = CARTESIAN_POINT ( 'NONE',  ( 4.171729424061789260, 46.82999999999999829, 12.83926296998457417 ) ) ;
#10932 = CARTESIAN_POINT ( 'NONE',  ( -13.49604125154532852, 70.91871731678214985, -0.3286502116883691649 ) ) ;
#10933 = CARTESIAN_POINT ( 'NONE',  ( -18.62500000000000000, -67.67499999999981242, -1.562973063126292757E-12 ) ) ;
#10934 = CARTESIAN_POINT ( 'NONE',  ( -5.633048038538731817, 67.38456837596503135, -12.26866196724357216 ) ) ;
#10935 = CARTESIAN_POINT ( 'NONE',  ( -1.564113515457998370E-12, -38.53749999999988063, 18.62500000000000000 ) ) ;
#10936 = CARTESIAN_POINT ( 'NONE',  ( 13.01147089442868499, 54.55850596185721457, -3.599127685514930342 ) ) ;
#10937 = EDGE_CURVE ( 'NONE', #546, #14568, #1114, .T. ) ;
#10938 = CARTESIAN_POINT ( 'NONE',  ( -11.53528178546093130, 64.66812037823611092, -7.019368641623308314 ) ) ;
#10939 = ORIENTED_EDGE ( 'NONE', *, *, #56, .F. ) ;
#10940 = CARTESIAN_POINT ( 'NONE',  ( 15.43600950528672477, 7.854010657973331533, -10.69176227072927432 ) ) ;
#10941 = CARTESIAN_POINT ( 'NONE',  ( -11.86977617365307225, 34.69196684977737277, -6.431069432459339374 ) ) ;
#10942 = ORIENTED_EDGE ( 'NONE', *, *, #2407, .F. ) ;
#10943 = CARTESIAN_POINT ( 'NONE',  ( 13.36905443401149540, 78.36436234710785698, 1.879137346049587487 ) ) ;
#10944 = CARTESIAN_POINT ( 'NONE',  ( 24.73863375370592976, 0.000000000000000000, 8.000000000000104805 ) ) ;
#10945 = CARTESIAN_POINT ( 'NONE',  ( -7.980211593510496471, 31.48200763573738570, -10.88882779094767983 ) ) ;
#10946 = CARTESIAN_POINT ( 'NONE',  ( 3.672445938696736967, 73.04794425685443571, -12.99169412694102199 ) ) ;
#10947 = CARTESIAN_POINT ( 'NONE',  ( 6.632128238234288986, 59.92444508611708898, 11.75866641223520759 ) ) ;
#10948 = CARTESIAN_POINT ( 'NONE',  ( -10.92172942406178926, -18.36999999999999744, -7.935100905948389460 ) ) ;
#10949 = CARTESIAN_POINT ( 'NONE',  ( 8.343458848123583849, 69.87999999999999545, -11.48378591275253768 ) ) ;
#10950 = CARTESIAN_POINT ( 'NONE',  ( -13.31348943002978125, 53.00938470406190106, 2.264923173904857201 ) ) ;
#10951 = B_SPLINE_CURVE_WITH_KNOTS ( 'NONE', 3,
 ( #11352, #14071, #3207, #4721, #9868, #1874, #564, #15218, #647, #3114, #10122, #1957, #7381, #12759, #8799, #477, #8542, #2044, #391, #11266, #12848, #11524, #10207, #15561, #3471, #2558, #10632, #6489, #10379, #3820, #3902, #13017, #11783, #9234, #898, #15997, #5160, #14409, #6310, #13190, #14324, #11872, #16987, #10465, #8968, #14670, #17335, #11696, #2213, #3642, #15826, #14588, #10552, #17072, #6575, #9320, #15733, #15911, #2468, #11611, #12930, #5246, #13276, #3730, #17247, #9056, #7901, #988, #11956, #7640, #814, #4976, #2297, #7725, #6225, #13101, #6400, #4891, #17159, #5071, #1164, #10292, #9148, #15644, #3554, #14495, #2382, #7818, #1075, #6922, #2821, #1414, #12299, #6657, #6831, #278, #5687, #17417, #16082, #5332, #10717, #5598, #11066, #3990, #1245, #4256, #13439, #2732, #8075, #9578, #1593, #13525, #13356, #9491, #15096, #13694, #12208, #10980, #9406, #102, #5507, #16440, #10890, #193, #1326, #7988, #16259, #4166, #12038, #6742, #14754, #2908, #14929, #2643, #8250, #12122, #16350, #13613, #1506, #9665, #11, #5415, #10804, #16166, #4342, #8338, #9751, #15016, #7010, #4076, #14838, #8160, #12387, #8515, #15276, #3089, #4608, #14131, #8600, #8425, #4521, #6034, #4435, #535, #1767, #5768, #12564, #12735, #711, #13952, #1933, #13865, #10184, #1849, #16702 ),
 .UNSPECIFIED., .F., .F.,
 ( 4, 2, 2, 2, 2, 1, 1, 2, 2, 2, 1, 2, 2, 2, 2, 2, 2, 1, 2, 2, 2, 2, 2, 2, 1, 1, 1, 1, 2, 2, 2, 1, 1, 1, 2, 2, 2, 2, 1, 2, 2, 2, 2, 2, 1, 2, 2, 1, 1, 1, 2, 2, 2, 1, 2, 2, 2, 2, 1, 2, 2, 1, 1, 2, 2, 2, 2, 1, 2, 2, 2, 1, 1, 1, 1, 1, 1, 1, 1, 2, 2, 2, 2, 2, 2, 2, 2, 1, 1, 2, 2, 2, 2, 2, 2, 2, 2, 2, 2, 1, 1, 1, 1, 2, 4 ),
 ( 0.5931508481644109931, 0.5940699344761732892, 0.5945294776320543262, 0.5945869205265394974, 0.5946156419737820276, 0.5946443634210246687, 0.5947592492099949002, 0.5949890207879354742, 0.5954485639438166222, 0.5956783355217571962, 0.5957932213107275388, 0.5958506642052125990, 0.5958793856524552401, 0.5959081070996977703, 0.5968271934114600663, 0.5970569649894006403, 0.5971144078838857006, 0.5971718507783708718, 0.5972867365673412143, 0.5977462797232223624, 0.5986653660349846584, 0.5995844523467469545, 0.5995988130703682195, 0.5996131737939895956, 0.5996418952412321257, 0.5996993381357172970, 0.5998142239246876395, 0.6000439955026282135, 0.6005035386585094725, 0.6014226249702718796, 0.6018821681261531387, 0.6019970539151234812, 0.6020544968096086524, 0.6020832182568511826, 0.6020975789804724476, 0.6021119397040937127, 0.6023417112820343977, 0.6041798839055592119, 0.6044096554834998969, 0.6045245412724701284, 0.6046394270614404709, 0.6050989702173216189, 0.6060180565290841370, 0.6069371428408465441, 0.6070520286298167756, 0.6071094715243019468, 0.6071381929715445880, 0.6071669144187871181, 0.6073966859967276921, 0.6078562291526089512, 0.6083157723084902102, 0.6083444937557327403, 0.6083732152029753815, 0.6084306580974604417, 0.6085455438864307842, 0.6087753154643713582, 0.6092348586202526173, 0.6094646301981931913, 0.6095795159871635338, 0.6096082374344060639, 0.6096225981580273290, 0.6096369588816485940, 0.6096944017761337653, 0.6115325743996586905, 0.6119921175555398385, 0.6121070033445101810, 0.6121644462389953523, 0.6122218891334805235, 0.6124516607114210975, 0.6133707470231835046, 0.6133994684704260347, 0.6134281899176685648, 0.6134856328121537361, 0.6136005186011240786, 0.6138302901790646526, 0.6142898333349458007, 0.6145196049128863747, 0.6145770478073715459, 0.6146057692546140760, 0.6146201299782353411, 0.6146344907018566062, 0.6147493764908269487, 0.6152089196467082077, 0.6161280059584706148, 0.6170470922702331329, 0.6171045351647183042, 0.6171332566119608343, 0.6171619780592034754, 0.6172768638481737069, 0.6175066354261143919, 0.6179661785819955400, 0.6188852648937579470, 0.6193448080496392061, 0.6195745796275797801, 0.6198043512055204651, 0.6207234375172828722, 0.6216425238290452793, 0.6221020669849264273, 0.6223318385628671123, 0.6224467243518373438, 0.6225041672463225151, 0.6225328886935651562, 0.6225472494171864213, 0.6225544297789969983, 0.6225616101408076863 ),
 .UNSPECIFIED. ) ;
#10952 = CARTESIAN_POINT ( 'NONE',  ( 2.272985001014427788E-15, 44.17999999999998550, -12.37355403259654985 ) ) ;
#10953 = CARTESIAN_POINT ( 'NONE',  ( -8.691771469529815392E-16, 67.68000000000000682, 14.19474002721660355 ) ) ;
#10954 = CARTESIAN_POINT ( 'NONE',  ( -15.43323788540784314, 8.055324194567102580, -9.314791131849441186 ) ) ;
#10955 = CARTESIAN_POINT ( 'NONE',  ( 11.90994820305756718, 69.66503421312197020, -6.356414413265706997 ) ) ;
#10956 = CARTESIAN_POINT ( 'NONE',  ( -13.39266229628177918, 37.86830100434433177, -1.771454170845632614 ) ) ;
#10957 = CARTESIAN_POINT ( 'NONE',  ( 13.31123005953295113, 36.35096708053784198, 2.249764498763733744 ) ) ;
#10958 = CARTESIAN_POINT ( 'NONE',  ( -13.16986379960055409, -34.30624999999993463, 13.16986379959834252 ) ) ;
#10959 = CARTESIAN_POINT ( 'NONE',  ( -8.405755648187358986, 74.35874387436902566, 10.56379513576823825 ) ) ;
#10960 = CARTESIAN_POINT ( 'NONE',  ( -13.49157297123065113, 76.94640455294563708, 0.4769767824848614723 ) ) ;
#10961 = DIRECTION ( 'NONE',  ( 0.000000000000000000, 0.000000000000000000, -1.000000000000000000 ) ) ;
#10962 = CARTESIAN_POINT ( 'NONE',  ( -19.00000000000001776, 7.773118517290098950, 1.732050807568674466 ) ) ;
#10963 = CARTESIAN_POINT ( 'NONE',  ( -10.79499759444871465, 80.92999999999997840, 5.634798678241480729 ) ) ;
#10964 = DIRECTION ( 'NONE',  ( -8.379555213223520053E-14, 0.000000000000000000, 1.000000000000000000 ) ) ;
#10965 = CARTESIAN_POINT ( 'NONE',  ( 7.272992578804308828, -1.020000000000005347, 10.01041549318726709 ) ) ;
#10966 = CARTESIAN_POINT ( 'NONE',  ( -7.272992578804307939, 50.47999999999999687, -10.01041549318727064 ) ) ;
#10967 = CARTESIAN_POINT ( 'NONE',  ( -8.343458848123576743, -16.52000000000000313, -11.48378591275254301 ) ) ;
#10968 = CARTESIAN_POINT ( 'NONE',  ( -17.32050807568884210, 0.000000000000000000, 7.999999999999840128 ) ) ;
#10969 = CARTESIAN_POINT ( 'NONE',  ( 12.17225613010915630, 75.21553104833439818, 5.838516313590356610 ) ) ;
#10970 = CARTESIAN_POINT ( 'NONE',  ( 3.055286883508066875, 9.636628673746404573E-15, -14.49864048043250797 ) ) ;
#10971 = CIRCLE ( 'NONE', #10138, 8.999999999999994671 ) ;
#10972 = CARTESIAN_POINT ( 'NONE',  ( 9.520470885617717371, 31.72999999999999332, -6.917026985038131848 ) ) ;
#10973 = CARTESIAN_POINT ( 'NONE',  ( -5.731539176755555687, 41.47177041787331575, 12.23222747491296403 ) ) ;
#10974 = CARTESIAN_POINT ( 'NONE',  ( -3.535167248572977261, 58.30710965717599947, -13.03526438387624964 ) ) ;
#10975 = CARTESIAN_POINT ( 'NONE',  ( 4.618812367767958449, 44.84625946610768921, 12.68529031168209009 ) ) ;
#10976 = CARTESIAN_POINT ( 'NONE',  ( -8.343458848123582072, 55.37999999999998835, 11.48378591275253768 ) ) ;
#10977 = CARTESIAN_POINT ( 'NONE',  ( 10.99999999999990941, 7.773118517290098062, 15.58845726811995824 ) ) ;
#10978 = CARTESIAN_POINT ( 'NONE',  ( -8.343458848123578520, 57.48000000000000398, -11.48378591275254124 ) ) ;
#10979 = EDGE_CURVE ( 'NONE', #4213, #10745, #14469, .T. ) ;
#10980 = CARTESIAN_POINT ( 'NONE',  ( -11.52230132989533651, 49.66675174565017414, -7.055497591694980919 ) ) ;
#10981 = CARTESIAN_POINT ( 'NONE',  ( 11.50794140772470442, 63.69349671364791021, -7.058136192068576342 ) ) ;
#10982 = CARTESIAN_POINT ( 'NONE',  ( 9.471282408482009529, 42.05193615182220412, 9.629884418960235948 ) ) ;
#10983 = CARTESIAN_POINT ( 'NONE',  ( 3.785595641572113985E-06, 49.17999986388394973, -13.49999999999946887 ) ) ;
#10984 = CIRCLE ( 'NONE', #3353, 1.999999999999997335 ) ;
#10985 = VERTEX_POINT ( 'NONE', #7885 ) ;
#10986 = CARTESIAN_POINT ( 'NONE',  ( -2.363332742774242767, 70.26497115792561488, -13.29196632392810429 ) ) ;
#10987 = CARTESIAN_POINT ( 'NONE',  ( -10.92172942406178926, 10.63000000000000078, -7.935100905948389460 ) ) ;
#10988 = ORIENTED_EDGE ( 'NONE', *, *, #2367, .F. ) ;
#10989 = CARTESIAN_POINT ( 'NONE',  ( -8.845124509614564090, 43.52173457442797400, -10.19943598800505846 ) ) ;
#10990 = CARTESIAN_POINT ( 'NONE',  ( 0.000000000000000000, 73.00000000000001421, -5.000000000000000000 ) ) ;
#10991 = CARTESIAN_POINT ( 'NONE',  ( 11.61166856071877795, 60.68652284347961512, -6.886578250901779441 ) ) ;
#10992 = SHAPE_REPRESENTATION ( 'Top rod', ( #16654 ), #5681 ) ;
#10993 = CARTESIAN_POINT ( 'NONE',  ( 13.50000000000000000, 7.429999999999992610, 1.734723475976807094E-15 ) ) ;
#10994 = FACE_OUTER_BOUND ( 'NONE', #14592, .T. ) ;
#10995 = CARTESIAN_POINT ( 'NONE',  ( 11.44624021849559270, 66.69747484006249749, -7.161096640856107420 ) ) ;
#10996 = CARTESIAN_POINT ( 'NONE',  ( 8.472248300915232733, 57.00428603186374232, 10.51143461932150736 ) ) ;
#10997 = CARTESIAN_POINT ( 'NONE',  ( 11.76794919243112680, 55.58000000000000540, -3.823638476888993942 ) ) ;
#10998 = CARTESIAN_POINT ( 'NONE',  ( 9.520470885617717371, 67.73000000000000398, -6.917026985038131848 ) ) ;
#10999 = CARTESIAN_POINT ( 'NONE',  ( -2.563398806372461536, 47.58790005324861738, 13.26025254451834456 ) ) ;
#11000 = FACE_BOUND ( 'NONE', #2132, .T. ) ;
#11001 = CARTESIAN_POINT ( 'NONE',  ( 13.49999999999999822, 74.28000000000000114, 4.386415899144236796 ) ) ;
#11002 = CARTESIAN_POINT ( 'NONE',  ( 18.08535795341810726, -99.99999999999998579, 4.251752263608082671 ) ) ;
#11003 = CARTESIAN_POINT ( 'NONE',  ( -8.050362892394746339, 10.00000000000000000, -9.725060096452381231 ) ) ;
#11004 = CARTESIAN_POINT ( 'NONE',  ( -11.37500000000039613, -75.96562499999980389, 4.711679271993002516 ) ) ;
#11005 = CARTESIAN_POINT ( 'NONE',  ( -4.171729424061791036, 52.53000000000000114, 12.83926296998457239 ) ) ;
#11006 = CARTESIAN_POINT ( 'NONE',  ( 13.48617201663203780, 33.45105711750449728, -0.6112691538384680268 ) ) ;
#11007 = CARTESIAN_POINT ( 'NONE',  ( -0.3072279589061667204, 9.999999999999998224, 12.93108829551862726 ) ) ;
#11008 = CARTESIAN_POINT ( 'NONE',  ( -8.774331155933998261, 8.058088662093549459, -15.73461071973920511 ) ) ;
#11009 = CARTESIAN_POINT ( 'NONE',  ( 11.76794919243112325, 23.43000000000000682, 1.734723475976807094E-15 ) ) ;
#11010 = ORIENTED_EDGE ( 'NONE', *, *, #10715, .F. ) ;
#11011 = CARTESIAN_POINT ( 'NONE',  ( -5.632579572119366773, 62.47544819939797378, 12.26882833910524617 ) ) ;
#11012 = EDGE_LOOP ( 'NONE', ( #1710, #10894, #15413, #13533 ) ) ;
#11013 = CARTESIAN_POINT ( 'NONE',  ( -13.32942039305800819, 41.00505323559917770, 2.139340077664309892 ) ) ;
#11014 = CARTESIAN_POINT ( 'NONE',  ( -18.62499999999935341, -64.48437499999987210, -7.714727599200458030 ) ) ;
#11015 = AXIS2_PLACEMENT_3D ( 'NONE', #16885, #3715, #2455 ) ;
#11016 = CARTESIAN_POINT ( 'NONE',  ( -13.47749323749192740, 43.95689747672926018, 0.7792445917878014772 ) ) ;
#11017 = DIRECTION ( 'NONE',  ( -1.000000000000000000, -1.445602896647338917E-16, 0.000000000000000000 ) ) ;
#11018 = CARTESIAN_POINT ( 'NONE',  ( 4.171729424061789260, 35.82999999999999119, 12.83926296998457417 ) ) ;
#11019 = CARTESIAN_POINT ( 'NONE',  ( 13.50000000000000355, 44.58000000000000540, -4.386415899144233244 ) ) ;
#11020 = CARTESIAN_POINT ( 'NONE',  ( -13.49688162372039990, 70.92003375154399691, -0.2904274958478991753 ) ) ;
#11021 = CARTESIAN_POINT ( 'NONE',  ( 18.62500000000000000, -26.04999999999992255, 1.560692158462880521E-12 ) ) ;
#11022 = CARTESIAN_POINT ( 'NONE',  ( -10.91250422740056614, 67.62945040754487991, -7.948069400918766902 ) ) ;
#11023 = CARTESIAN_POINT ( 'NONE',  ( 18.62500000000064659, -43.74062499999988773, -7.714727599197336083 ) ) ;
#11024 = EDGE_CURVE ( 'NONE', #7559, #16001, #7804, .T. ) ;
#11025 = CARTESIAN_POINT ( 'NONE',  ( 13.42879437376425500, 54.37163056846146247, 1.680570053129028629 ) ) ;
#11026 = CARTESIAN_POINT ( 'NONE',  ( -2.624842932224632719, 64.27450954149531981, -13.24583211552917739 ) ) ;
#11027 = EDGE_LOOP ( 'NONE', ( #6664, #4301, #12651, #2959 ) ) ;
#11028 = CARTESIAN_POINT ( 'NONE',  ( -11.85197915507875521, 34.69064970905623824, -6.463791718503999917 ) ) ;
#11029 = VERTEX_POINT ( 'NONE', #10278 ) ;
#11030 = CARTESIAN_POINT ( 'NONE',  ( 13.42225261468230713, 78.37947749321138247, 1.448575772764510328 ) ) ;
#11031 = CARTESIAN_POINT ( 'NONE',  ( -13.35468963145571841, 1.171226224988986705E-15, -0.4314527491507029744 ) ) ;
#11032 = CARTESIAN_POINT ( 'NONE',  ( 24.73863375370592976, 5.918584287042170544, 8.000000000000106581 ) ) ;
#11033 = CARTESIAN_POINT ( 'NONE',  ( 7.500000000000002665, -23.27176790847081023, 9.199276322163095543 ) ) ;
#11034 = CARTESIAN_POINT ( 'NONE',  ( 11.20647886694230522, 72.71291404450818163, -7.527623646720101647 ) ) ;
#11035 = CARTESIAN_POINT ( 'NONE',  ( 0.03691118140029227973, 79.17867285846638481, -13.49996200175932692 ) ) ;
#11036 = CARTESIAN_POINT ( 'NONE',  ( 8.343458848123583849, -19.12000000000000455, -11.48378591275253768 ) ) ;
#11037 = CARTESIAN_POINT ( 'NONE',  ( 4.171729424061791924, 73.03000000000000114, -12.83926296998457239 ) ) ;
#11038 = CARTESIAN_POINT ( 'NONE',  ( -11.20932835276732575, 52.64727559639315757, -7.523361188747804462 ) ) ;
#11039 = ADVANCED_FACE ( 'NONE', ( #8952, #10536 ), #14394, .F. ) ;
#11040 = CARTESIAN_POINT ( 'NONE',  ( -11.76794919243112325, 44.77999999999998693, -3.823638476888998827 ) ) ;
#11041 = CARTESIAN_POINT ( 'NONE',  ( -7.272992578804307939, -17.52000000000000313, -10.01041549318726886 ) ) ;
#11042 = CARTESIAN_POINT ( 'NONE',  ( 0.4447399503994752812, 50.69609182596189356, 13.49999999964396302 ) ) ;
#11043 = CARTESIAN_POINT ( 'NONE',  ( 11.07943945917226181, 69.13930839722881672, 7.714844222956088515 ) ) ;
#11044 = CARTESIAN_POINT ( 'NONE',  ( 10.00000000000002132, 0.000000000000000000, -15.32050807568876394 ) ) ;
#11045 = CARTESIAN_POINT ( 'NONE',  ( -7.379696451821980833E-14, 6.046025403784444308, -12.00000000000000000 ) ) ;
#11046 = CARTESIAN_POINT ( 'NONE',  ( 13.16986379959833897, -55.11874999999988489, 13.16986379960055409 ) ) ;
#11047 = CARTESIAN_POINT ( 'NONE',  ( -13.12364411654131402, 74.04252074095533942, 3.167980043827653525 ) ) ;
#11048 = CARTESIAN_POINT ( 'NONE',  ( -8.341416350532403712, 76.49767382419285866, -10.64073998737741533 ) ) ;
#11049 = CARTESIAN_POINT ( 'NONE',  ( -4.085520694688061560, 79.32684323223975298, -12.86729062109435340 ) ) ;
#11050 = CARTESIAN_POINT ( 'NONE',  ( 0.000000000000000000, 0.000000000000000000, 12.00000000000000178 ) ) ;
#11051 = CARTESIAN_POINT ( 'NONE',  ( 13.50000000000000355, 4.580000000000007176, -4.386415899144233244 ) ) ;
#11052 = SURFACE_STYLE_USAGE ( .BOTH. , #264 ) ;
#11053 = CARTESIAN_POINT ( 'NONE',  ( 7.272992578804308828, -10.02000000000000490, 10.01041549318726709 ) ) ;
#11054 = CARTESIAN_POINT ( 'NONE',  ( 7.272992578804308828, 51.97999999999998977, 10.01041549318726886 ) ) ;
#11055 = CARTESIAN_POINT ( 'NONE',  ( -8.343458848123576743, -13.52000000000000135, -11.48378591275254301 ) ) ;
#11056 = CARTESIAN_POINT ( 'NONE',  ( -4.494282199184345572, 32.51830724862094257, 12.72999398840573448 ) ) ;
#11057 = CARTESIAN_POINT ( 'NONE',  ( 13.47046671447611921, 75.39302779519800879, 1.059546044154582312 ) ) ;
#11058 = CARTESIAN_POINT ( 'NONE',  ( 8.887463110696979030, -7.486575357575272229E-16, -7.985952341615979222 ) ) ;
#11059 = CARTESIAN_POINT ( 'NONE',  ( 9.520470885617715595, 34.13000000000000256, 6.917026985038134512 ) ) ;
#11060 = CARTESIAN_POINT ( 'NONE',  ( -12.54844231482822003, 41.11082418795689364, 4.978620826851912540 ) ) ;
#11061 = CARTESIAN_POINT ( 'NONE',  ( -2.347235880096729677, 58.26439793459769589, -13.29438112138644712 ) ) ;
#11062 = DIRECTION ( 'NONE',  ( 0.000000000000000000, 0.000000000000000000, -1.000000000000000000 ) ) ;
#11063 = FACE_OUTER_BOUND ( 'NONE', #11099, .T. ) ;
#11064 = CARTESIAN_POINT ( 'NONE',  ( 16.82677684650024474, 7.170662809914417402, 13.14483242576222821 ) ) ;
#11065 = CARTESIAN_POINT ( 'NONE',  ( -0.5497339802477337889, 55.19976638620128995, -13.48880876228390591 ) ) ;
#11066 = CARTESIAN_POINT ( 'NONE',  ( -13.26384252841972966, 49.84140379325150150, -2.514066362863750292 ) ) ;
#11067 = AXIS2_PLACEMENT_3D ( 'NONE', #9310, #6477, #12112 ) ;
#11068 = CARTESIAN_POINT ( 'NONE',  ( 10.38695722535535104, 63.09982902898799040, 8.626549733017945698 ) ) ;
#11069 = CARTESIAN_POINT ( 'NONE',  ( 13.48620919108931382, 42.40890622764071338, 0.6106556734208694603 ) ) ;
#11070 = CARTESIAN_POINT ( 'NONE',  ( -18.11581985354938951, 8.027799059190092734, 0.6932941240385166459 ) ) ;
#11071 = ORIENTED_EDGE ( 'NONE', *, *, #13672, .F. ) ;
#11072 = CARTESIAN_POINT ( 'NONE',  ( -11.76794919243112325, 72.07999999999999829, 3.823638476888994830 ) ) ;
#11073 = CARTESIAN_POINT ( 'NONE',  ( -4.128382448430371277, 70.32844985923892978, -12.85360630656942504 ) ) ;
#11074 = CARTESIAN_POINT ( 'NONE',  ( -11.37500000000039613, -75.96562499999981810, 4.711679271993001628 ) ) ;
#11075 = CARTESIAN_POINT ( 'NONE',  ( 8.343458848123583849, 9.879999999999999005, -11.48378591275253768 ) ) ;
#11076 = VERTEX_POINT ( 'NONE', #15720 ) ;
#11077 = CARTESIAN_POINT ( 'NONE',  ( -2.247839795003510055, 43.26082400849369947, -13.31154558271445509 ) ) ;
#11078 = CARTESIAN_POINT ( 'NONE',  ( -7.500000000000000000, 106.5806336763438935, 7.726132535793189149 ) ) ;
#11079 = CARTESIAN_POINT ( 'NONE',  ( 6.401920825618216959, 60.94496828387899257, -11.88551464368857680 ) ) ;
#11080 = CARTESIAN_POINT ( 'NONE',  ( -8.343458848123582072, 3.380000000000000338, 11.48378591275254124 ) ) ;
#11081 = CARTESIAN_POINT ( 'NONE',  ( 18.62500000000064304, -1.040624999999997469, -7.714727599197334307 ) ) ;
#11082 = CARTESIAN_POINT ( 'NONE',  ( 13.25906685095921489, 66.33919486957000800, 2.577579219623620244 ) ) ;
#11083 = CARTESIAN_POINT ( 'NONE',  ( 1.401137238041307853, 56.73038022015892778, 13.42714289984223797 ) ) ;
#11084 = EDGE_CURVE ( 'NONE', #11880, #16659, #3439, .T. ) ;
#11085 = CARTESIAN_POINT ( 'NONE',  ( -7.576616670048093940E-16, 57.67999999999999261, 12.37355403259654985 ) ) ;
#11086 = CARTESIAN_POINT ( 'NONE',  ( 2.272985001014427788E-15, 68.18000000000000682, -12.37355403259654985 ) ) ;
#11087 = AXIS2_PLACEMENT_3D ( 'NONE', #15664, #15492, #10056 ) ;
#11088 = CARTESIAN_POINT ( 'NONE',  ( -13.24853700240426058, 46.83817720085215086, -2.602182145016867842 ) ) ;
#11089 = PLANE ( 'NONE',  #15181 ) ;
#11090 = CARTESIAN_POINT ( 'NONE',  ( 7.312260103668256263E-16, 8.062177826491094379, -18.00000000000000000 ) ) ;
#11091 = CARTESIAN_POINT ( 'NONE',  ( 11.26921262112964683, 30.70896170274106396, -7.433369082940963324 ) ) ;
#11092 = CARTESIAN_POINT ( 'NONE',  ( -8.617953050394065784, 56.34892783574404262, 10.39139140008484574 ) ) ;
#11093 = CARTESIAN_POINT ( 'NONE',  ( 4.711679271994909435, -53.07187499999987068, -11.37499999999960387 ) ) ;
#11094 = DIRECTION ( 'NONE',  ( -1.000000000000000000, -1.734723475976807094E-16, -0.000000000000000000 ) ) ;
#11095 = CARTESIAN_POINT ( 'NONE',  ( 6.741542013777170439, 32.92885702970292527, 11.69833832118984773 ) ) ;
#11096 = CARTESIAN_POINT ( 'NONE',  ( -8.056527170155236561, 10.00000000000000355, 9.383171173929708786 ) ) ;
#11097 = CARTESIAN_POINT ( 'NONE',  ( 1.287047813695933574, 40.13382801857486015, -13.44065531857610019 ) ) ;
#11098 = ORIENTED_EDGE ( 'NONE', *, *, #10503, .T. ) ;
#11099 = EDGE_LOOP ( 'NONE', ( #9761, #9413, #16357, #4105 ) ) ;
#11100 = AXIS2_PLACEMENT_3D ( 'NONE', #10102, #8778, #14134 ) ;
#11101 = CARTESIAN_POINT ( 'NONE',  ( 13.16986379959833897, -55.11874999999988489, 13.16986379960055409 ) ) ;
#11102 = CARTESIAN_POINT ( 'NONE',  ( -13.49677891199997504, 43.94321173900256383, 0.3859101346687785483 ) ) ;
#11103 = DIRECTION ( 'NONE',  ( 0.000000000000000000, 0.000000000000000000, 1.000000000000000000 ) ) ;
#11104 = CARTESIAN_POINT ( 'NONE',  ( -4.171729424061791036, 35.53000000000000114, 12.83926296998457239 ) ) ;
#11105 = ADVANCED_FACE ( 'NONE', ( #3807 ), #15811, .T. ) ;
#11106 = AXIS2_PLACEMENT_3D ( 'NONE', #844, #14445, #12792 ) ;
#11107 = CARTESIAN_POINT ( 'NONE',  ( -6.314785314735273047, 46.41152104994968397, -11.93203815175650462 ) ) ;
#11108 = CARTESIAN_POINT ( 'NONE',  ( -11.69000891540406073, 67.67898000483805276, -6.752419532946158931 ) ) ;
#11109 = CARTESIAN_POINT ( 'NONE',  ( -13.16986379959834252, -48.94374999999985931, -13.16986379960055409 ) ) ;
#11110 = CARTESIAN_POINT ( 'NONE',  ( 11.73858346217181037, 54.18242075136932812, 6.667783194025956206 ) ) ;
#11111 = CARTESIAN_POINT ( 'NONE',  ( 2.279995255611139653E-15, 15.18000000000000504, -12.37355403259654985 ) ) ;
#11112 = CARTESIAN_POINT ( 'NONE',  ( -5.878827033754383535, 64.39416732176437108, -12.15275301167633870 ) ) ;
#11113 = EDGE_LOOP ( 'NONE', ( #697, #6952, #1085, #15282 ) ) ;
#11114 = CARTESIAN_POINT ( 'NONE',  ( -11.47022446788024830, 35.19602096309857586, 7.119919174184125232 ) ) ;
#11115 = ORIENTED_EDGE ( 'NONE', *, *, #2530, .T. ) ;
#11116 = CARTESIAN_POINT ( 'NONE',  ( 11.71436862115008637, 78.18064915872857057, 6.711522305461322446 ) ) ;
#11117 = CARTESIAN_POINT ( 'NONE',  ( -9.999999999999776179, 7.983052681820796970, -15.32050807568890427 ) ) ;
#11118 = CARTESIAN_POINT ( 'NONE',  ( 7.500000000000000000, -22.51433466932076755, -9.346209313438661681 ) ) ;
#11119 = CARTESIAN_POINT ( 'NONE',  ( 4.654787199579893731, 73.01242072379346837, -12.67213584933875836 ) ) ;
#11120 = CARTESIAN_POINT ( 'NONE',  ( 2.519697212011065446, 79.08940101069002537, -13.26277544837490296 ) ) ;
#11121 = CARTESIAN_POINT ( 'NONE',  ( -10.92172942406178926, -12.36999999999999922, -7.935100905948389460 ) ) ;
#11122 = CARTESIAN_POINT ( 'NONE',  ( -8.343458848123582072, 62.37999999999998835, 11.48378591275254124 ) ) ;
#11123 = CARTESIAN_POINT ( 'NONE',  ( 13.50000000000000355, 50.58000000000000540, -4.386415899144233244 ) ) ;
#11124 = CARTESIAN_POINT ( 'NONE',  ( -13.50515042037184976, 52.92788077079702447, -0.05679620317202376673 ) ) ;
#11125 = EDGE_CURVE ( 'NONE', #8460, #11876, #3539, .T. ) ;
#11126 = CARTESIAN_POINT ( 'NONE',  ( -11.76794919243112325, 41.77999999999999403, -3.823638476888998827 ) ) ;
#11127 = CARTESIAN_POINT ( 'NONE',  ( 11.76794919243112325, -18.56999999999999673, 1.734723475976807094E-15 ) ) ;
#11128 = CARTESIAN_POINT ( 'NONE',  ( -4.171729424061791036, 58.53000000000000114, 12.83926296998457239 ) ) ;
#11129 = CARTESIAN_POINT ( 'NONE',  ( 1.564284005194032989, 50.73624596681315779, 13.40908526793743505 ) ) ;
#11130 = B_SPLINE_CURVE_WITH_KNOTS ( 'NONE', 3,
 ( #6242, #2317, #2229, #1093 ),
 .UNSPECIFIED., .F., .F.,
 ( 4, 4 ),
 ( 2.376698214939480797E-07, 0.007646667280170309916 ),
 .UNSPECIFIED. ) ;
#11131 = CARTESIAN_POINT ( 'NONE',  ( 10.96292031448879989, 69.13240560544066682, 7.878467101911673431 ) ) ;
#11132 = CARTESIAN_POINT ( 'NONE',  ( 6.750022862106053623, 29.92926176209967437, 11.69132975161703669 ) ) ;
#11133 = CARTESIAN_POINT ( 'NONE',  ( 0.4450047276655222372, 35.69605895621225500, 13.49999999987117683 ) ) ;
#11134 = CARTESIAN_POINT ( 'NONE',  ( -7.714727599200466912, -85.29687499999984368, 18.62499999999935341 ) ) ;
#11135 = CARTESIAN_POINT ( 'NONE',  ( -10.07304411609868922, 74.27699509055480576, 8.989944076744466273 ) ) ;
#11136 = CARTESIAN_POINT ( 'NONE',  ( -7.164914557665265527, 76.44660487377331037, -11.44177756266805268 ) ) ;
#11137 = CARTESIAN_POINT ( 'NONE',  ( 0.000000000000000000, 80.93000000000000682, 0.000000000000000000 ) ) ;
#11138 = DIRECTION ( 'NONE',  ( -1.224646799147353207E-16, 0.000000000000000000, -1.000000000000000000 ) ) ;
#11139 = CARTESIAN_POINT ( 'NONE',  ( -3.636496289402152637, -8.669999999999996376, -11.19198476289190936 ) ) ;
#11140 = CARTESIAN_POINT ( 'NONE',  ( 3.636496289402157078, 41.02999999999999403, -11.19198476289190936 ) ) ;
#11141 = CARTESIAN_POINT ( 'NONE',  ( 8.343458848123583849, -14.12000000000000455, -11.48378591275253768 ) ) ;
#11142 = CARTESIAN_POINT ( 'NONE',  ( -7.134497763750654364, 32.41468128586360820, 11.46076502362460836 ) ) ;
#11143 = CARTESIAN_POINT ( 'NONE',  ( 13.32613498935721807, 75.35421527273051368, 2.159664486192276467 ) ) ;
#11144 = CARTESIAN_POINT ( 'NONE',  ( 17.16739154622002062, 3.710240846040480518E-14, -6.862782679473228065 ) ) ;
#11145 = CARTESIAN_POINT ( 'NONE',  ( 9.520470885617715595, 31.12999999999999901, 6.917026985038134512 ) ) ;
#11146 = CARTESIAN_POINT ( 'NONE',  ( -13.49999999999999822, 82.08000000000001251, 4.386415899144235908 ) ) ;
#11147 = CIRCLE ( 'NONE', #2935, 26.00000000000000355 ) ;
#11148 = CARTESIAN_POINT ( 'NONE',  ( 7.620118401036991784, 51.89386994708977596, -11.14470155242018912 ) ) ;
#11149 = CARTESIAN_POINT ( 'NONE',  ( -0.4450088281291025294, 38.66413328918902437, 13.50000000012805756 ) ) ;
#11150 = CARTESIAN_POINT ( 'NONE',  ( 0.7721810585093080714, 37.15227321576206521, -13.48105077863768742 ) ) ;
#11151 = DIRECTION ( 'NONE',  ( -0.000000000000000000, 1.000000000000000000, -0.000000000000000000 ) ) ;
#11152 = DIRECTION ( 'NONE',  ( 0.000000000000000000, 1.000000000000000000, 0.000000000000000000 ) ) ;
#11153 = CARTESIAN_POINT ( 'NONE',  ( 7.321132905710702410, 62.95323300269863154, 11.34287645249957777 ) ) ;
#11154 = CARTESIAN_POINT ( 'NONE',  ( 13.48357555260946228, 42.45296674144867666, -0.6662799819680408353 ) ) ;
#11155 = CARTESIAN_POINT ( 'NONE',  ( 6.511591735624385535, 48.94067668905481838, -11.83699345231539546 ) ) ;
#11156 = CARTESIAN_POINT ( 'NONE',  ( 7.272992578804311492, 20.87999999999999545, -10.01041549318726709 ) ) ;
#11157 = EDGE_CURVE ( 'NONE', #17140, #11029, #7129, .T. ) ;
#11158 = ORIENTED_EDGE ( 'NONE', *, *, #13269, .T. ) ;
#11159 = CARTESIAN_POINT ( 'NONE',  ( -7.272992578804310604, 63.37999999999999545, 10.01041549318726886 ) ) ;
#11160 = CARTESIAN_POINT ( 'NONE',  ( -0.5895600827330491622, 70.20119840546840351, -13.49999998549911773 ) ) ;
#11161 = CARTESIAN_POINT ( 'NONE',  ( -8.043339635997654113, -60.35624999999985363, 8.043339635996302306 ) ) ;
#11162 = CARTESIAN_POINT ( 'NONE',  ( 4.171729424061791924, 4.030000000000005578, -12.83926296998457239 ) ) ;
#11163 = EDGE_LOOP ( 'NONE', ( #7308, #16882, #15715, #9244 ) ) ;
#11164 = CARTESIAN_POINT ( 'NONE',  ( -8.945013995349350822, 43.52648452866512230, -10.11178031813171785 ) ) ;
#11165 = CARTESIAN_POINT ( 'NONE',  ( -7.500000000000000000, 108.6229112031126505, -2.544524385544284062 ) ) ;
#11166 = CARTESIAN_POINT ( 'NONE',  ( 6.420329193139213686, 60.94422300306127482, -11.87558703656385184 ) ) ;
#11167 = CARTESIAN_POINT ( 'NONE',  ( 13.50000000000000355, 4.580000000000007176, -4.386415899144233244 ) ) ;
#11168 = CARTESIAN_POINT ( 'NONE',  ( 3.708203932499371192, 0.1639745962155645387, -11.41267819554184371 ) ) ;
#11169 = CARTESIAN_POINT ( 'NONE',  ( -1.900613283894470484, 6.122906826104709488, -11.99999999999998934 ) ) ;
#11170 = CARTESIAN_POINT ( 'NONE',  ( 9.980110855971577877, 66.07825710158466848, 9.092675784874080236 ) ) ;
#11171 = CARTESIAN_POINT ( 'NONE',  ( 11.01769831327593074, 57.13567825725026950, 7.805250006001219987 ) ) ;
#11172 = CARTESIAN_POINT ( 'NONE',  ( -7.272992578804310604, 63.37999999999998835, 10.01041549318726709 ) ) ;
#11173 = CARTESIAN_POINT ( 'NONE',  ( -4.171729424061787483, 33.32999999999999829, -12.83926296998457417 ) ) ;
#11174 = CARTESIAN_POINT ( 'NONE',  ( 3.636496289402157078, 71.03000000000000114, -11.19198476289190936 ) ) ;
#11175 = CARTESIAN_POINT ( 'NONE',  ( -13.31651195430729828, 46.85210362530030892, -2.218283652183269172 ) ) ;
#11176 = CARTESIAN_POINT ( 'NONE',  ( 8.201072769536251528, 45.86863449535839266, -10.74934398742807495 ) ) ;
#11177 = CARTESIAN_POINT ( 'NONE',  ( 1.732050807568877415, 7.773118517290098950, -19.00000000000000000 ) ) ;
#11178 = CARTESIAN_POINT ( 'NONE',  ( 8.348315818218853934, 30.86137531282033208, -10.60922870909750593 ) ) ;
#11179 = CARTESIAN_POINT ( 'NONE',  ( -5.838732723835591720, 56.46738623871877394, 12.17296727378241350 ) ) ;
#11180 = CARTESIAN_POINT ( 'NONE',  ( 11.37500000000039435, -84.29062499999983515, -4.711679271993004292 ) ) ;
#11181 = DIRECTION ( 'NONE',  ( 0.000000000000000000, -1.000000000000000000, 0.000000000000000000 ) ) ;
#11182 = CARTESIAN_POINT ( 'NONE',  ( 10.96333157205655873, 33.13238853848653775, 7.878424145257830524 ) ) ;
#11183 = CARTESIAN_POINT ( 'NONE',  ( -8.891200544363830713E-16, 4.546025403784440755, 12.00000000000000000 ) ) ;
#11184 = CARTESIAN_POINT ( 'NONE',  ( 3.273252351246041414, 40.06251456520496390, -13.10396545777065747 ) ) ;
#11185 = EDGE_CURVE ( 'NONE', #16216, #16109, #13906, .T. ) ;
#11186 = EDGE_LOOP ( 'NONE', ( #17424, #286, #16398, #4174 ) ) ;
#11187 = CARTESIAN_POINT ( 'NONE',  ( -10.11974732110556374, 62.27491796265164226, 8.946316878496988423 ) ) ;
#11188 = VECTOR ( 'NONE', #10147, 1000.000000000000000 ) ;
#11189 = ORIENTED_EDGE ( 'NONE', *, *, #3486, .T. ) ;
#11190 = CARTESIAN_POINT ( 'NONE',  ( 13.16986379960055409, -75.93124999999983515, -13.16986379959834430 ) ) ;
#11191 = CARTESIAN_POINT ( 'NONE',  ( -11.11006920932890196, 44.21883285313256806, 7.669478262804471314 ) ) ;
#11192 = CYLINDRICAL_SURFACE ( 'NONE', #1707, 13.50000000000000000 ) ;
#11193 = CARTESIAN_POINT ( 'NONE',  ( 10.92172942406178926, 36.12999999999999545, 7.935100905948387684 ) ) ;
#11194 = CARTESIAN_POINT ( 'NONE',  ( 10.92172942406179104, 47.73000000000000398, -7.935100905948385908 ) ) ;
#11195 = AXIS2_PLACEMENT_3D ( 'NONE', #12733, #8773, #2993 ) ;
#11196 = CARTESIAN_POINT ( 'NONE',  ( -8.219743528356605822, 46.49234792102033964, -10.74582137773523449 ) ) ;
#11197 = CARTESIAN_POINT ( 'NONE',  ( -7.992194457595993562, 67.48253745615919286, -10.88025959043272373 ) ) ;
#11198 = CARTESIAN_POINT ( 'NONE',  ( -7.714727599200466912, -37.49687499999989626, 18.62499999999935341 ) ) ;
#11199 = CARTESIAN_POINT ( 'NONE',  ( 9.413837210981146342, 54.04933858495957111, 9.676282647599792952 ) ) ;
#11200 = CARTESIAN_POINT ( 'NONE',  ( -8.082238262464676026, 64.48655149555420962, -10.81439697735142502 ) ) ;
#11201 = EDGE_CURVE ( 'NONE', #2220, #5991, #5493, .T. ) ;
#11202 = ORIENTED_EDGE ( 'NONE', *, *, #4672, .T. ) ;
#11203 = CARTESIAN_POINT ( 'NONE',  ( -10.37171067933893376, 34.59884894902187824, -8.642314730309303528 ) ) ;
#11204 = CARTESIAN_POINT ( 'NONE',  ( 8.043339635997654113, -68.68124999999983515, -8.043339635996304082 ) ) ;
#11205 = CARTESIAN_POINT ( 'NONE',  ( 13.47859327190760759, 78.39933782603816326, 0.8769525335675483202 ) ) ;
#11206 = CARTESIAN_POINT ( 'NONE',  ( -15.34211313687887923, 8.027799056124987231, 9.658320279281683796 ) ) ;
#11207 = AXIS2_PLACEMENT_3D ( 'NONE', #13379, #2403, #14693 ) ;
#11208 = CARTESIAN_POINT ( 'NONE',  ( 7.500000000000000888, -27.69291120311264365, -2.544524385544279177 ) ) ;
#11209 = CARTESIAN_POINT ( 'NONE',  ( 11.97746557486279251, 72.19970894202896261, 6.240527775782743092 ) ) ;
#11210 = CARTESIAN_POINT ( 'NONE',  ( 13.50000000000000355, -19.42000000000000171, -4.386415899144233244 ) ) ;
#11211 = CARTESIAN_POINT ( 'NONE',  ( -4.171729424061787483, 64.32999999999999829, -12.83926296998457417 ) ) ;
#11212 = CARTESIAN_POINT ( 'NONE',  ( -0.6196722084519333817, 71.65772062913328000, 13.48668984471889587 ) ) ;
#11213 = CARTESIAN_POINT ( 'NONE',  ( -7.272992578804307939, 35.47999999999999687, -10.01041549318726886 ) ) ;
#11214 = CARTESIAN_POINT ( 'NONE',  ( -10.92172942406178926, 54.62999999999999545, -7.935100905948389460 ) ) ;
#11215 = DIRECTION ( 'NONE',  ( 0.000000000000000000, 0.000000000000000000, -1.000000000000000000 ) ) ;
#11216 = CARTESIAN_POINT ( 'NONE',  ( -11.76794919243112325, 0.9300000000000141487, -2.602085213965210642E-15 ) ) ;
#11217 = CARTESIAN_POINT ( 'NONE',  ( 3.549402833027860638, 68.80762806818306387, 13.02504335811066305 ) ) ;
#11218 = CARTESIAN_POINT ( 'NONE',  ( 13.16986379960055054, -2.081249999999994937, -13.16986379959834430 ) ) ;
#11219 = CARTESIAN_POINT ( 'NONE',  ( -8.343458848123582072, 79.37999999999999545, 11.48378591275253768 ) ) ;
#11220 = CARTESIAN_POINT ( 'NONE',  ( -18.62499999999935341, -97.78437499999979821, -7.714727599200458030 ) ) ;
#11221 = CARTESIAN_POINT ( 'NONE',  ( -11.44226849560644155, 73.66214175551372989, -7.164337856285095896 ) ) ;
#11222 = CARTESIAN_POINT ( 'NONE',  ( -1.931361406942186720, 76.24943241617928891, -13.36225245988610588 ) ) ;
#11223 = ADVANCED_FACE ( 'NONE', ( #2718 ), #16496, .F. ) ;
#11224 = CARTESIAN_POINT ( 'NONE',  ( -0.8575635061788702274, 8.007388461842872118, -18.18484536092591242 ) ) ;
#11225 = CARTESIAN_POINT ( 'NONE',  ( -23.28534784291404591, 6.548267719634617734, 4.206197538246222223 ) ) ;
#11226 = DIRECTION ( 'NONE',  ( 0.000000000000000000, 0.000000000000000000, 1.000000000000000000 ) ) ;
#11227 = CARTESIAN_POINT ( 'NONE',  ( -8.343458848123576743, 32.47999999999999687, -11.48378591275254301 ) ) ;
#11228 = CARTESIAN_POINT ( 'NONE',  ( -7.409984580736203970E-16, -10.32000000000000384, 12.37355403259654985 ) ) ;
#11229 = CARTESIAN_POINT ( 'NONE',  ( 11.76794919243112325, 37.42999999999999972, 1.441158131103945434E-15 ) ) ;
#11230 = CARTESIAN_POINT ( 'NONE',  ( -8.343458848123582072, 2.380000000000003002, 11.48378591275253768 ) ) ;
#11231 = CARTESIAN_POINT ( 'NONE',  ( -4.425713338080228709, 32.52081085309985298, 12.75399470283292658 ) ) ;
#11232 = CARTESIAN_POINT ( 'NONE',  ( 1.295514318413480082, 74.72657971910703623, 13.43770740680674969 ) ) ;
#11233 = CARTESIAN_POINT ( 'NONE',  ( 12.31824352683052304, -2.318222727469660658E-13, -13.04685550568140329 ) ) ;
#11234 = CARTESIAN_POINT ( 'NONE',  ( 7.272992578804311492, 31.87999999999999545, -10.01041549318726709 ) ) ;
#11235 = CARTESIAN_POINT ( 'NONE',  ( -2.383599452370637195, 58.26570543616674058, -13.28790837415479231 ) ) ;
#11236 = DIRECTION ( 'NONE',  ( -0.000000000000000000, -1.000000000000000000, -0.000000000000000000 ) ) ;
#11237 = CARTESIAN_POINT ( 'NONE',  ( -8.891200544363830713E-16, 7.546025403784439867, 12.00000000000000000 ) ) ;
#11238 = DIRECTION ( 'NONE',  ( -0.4999999999999953371, 0.000000000000000000, -0.8660254037844412611 ) ) ;
#11239 = CARTESIAN_POINT ( 'NONE',  ( -11.88920123096388792, 9.999999999999994671, -1.626927807140451154 ) ) ;
#11240 = CARTESIAN_POINT ( 'NONE',  ( 11.55360894227645474, 63.16957824287888457, 6.983155331944742805 ) ) ;
#11241 = CARTESIAN_POINT ( 'NONE',  ( 13.46927589499868816, 42.39849010613973235, 0.9131328280806061404 ) ) ;
#11242 = CARTESIAN_POINT ( 'NONE',  ( 11.79887646993529948, 48.67349572257840862, -6.571923756045907616 ) ) ;
#11243 = CARTESIAN_POINT ( 'NONE',  ( -7.409984580736203970E-16, 25.67999999999999616, 12.37355403259654985 ) ) ;
#11244 = ORIENTED_EDGE ( 'NONE', *, *, #17031, .T. ) ;
#11245 = CARTESIAN_POINT ( 'NONE',  ( 2.272985001014427393E-15, 71.17999999999999261, -12.37355403259654807 ) ) ;
#11246 = CARTESIAN_POINT ( 'NONE',  ( 11.37500000000039613, 6.209375000000004974, -4.711679271993004292 ) ) ;
#11247 = CARTESIAN_POINT ( 'NONE',  ( -4.711679271994915652, -78.04687499999982947, 11.37499999999960210 ) ) ;
#11248 = CARTESIAN_POINT ( 'NONE',  ( 4.171729424061791924, 10.03000000000001180, -12.83926296998457239 ) ) ;
#11249 = ORIENTED_EDGE ( 'NONE', *, *, #7589, .F. ) ;
#11250 = CARTESIAN_POINT ( 'NONE',  ( 0.000000000000000000, 9.000000000000000000, -12.00000000000000178 ) ) ;
#11251 = CARTESIAN_POINT ( 'NONE',  ( -7.499999999999999112, 108.4800942032927509, -3.560038493048083730 ) ) ;
#11252 = CARTESIAN_POINT ( 'NONE',  ( -8.343458848123582072, 6.380000000000007887, 11.48378591275254124 ) ) ;
#11253 = CARTESIAN_POINT ( 'NONE',  ( -1.732050807568877859, 0.000000000000000000, -18.99999999999999645 ) ) ;
#11254 = CARTESIAN_POINT ( 'NONE',  ( 13.14794202937746093, 66.31858931631785481, 3.143476922865568568 ) ) ;
#11255 = CARTESIAN_POINT ( 'NONE',  ( 4.440672829457194659, 56.83962754305976262, 12.75201459754448230 ) ) ;
#11256 = CARTESIAN_POINT ( 'NONE',  ( -11.76794919243112325, 57.07999999999999829, 3.823638476888994386 ) ) ;
#11257 = CARTESIAN_POINT ( 'NONE',  ( 10.92172942406178926, 32.12999999999999545, 7.935100905948387684 ) ) ;
#11258 = CARTESIAN_POINT ( 'NONE',  ( 7.272992578804311492, 70.87999999999998124, -10.01041549318726709 ) ) ;
#11259 = CARTESIAN_POINT ( 'NONE',  ( -11.32938012359942981, 46.65483419514092844, -7.341333998329178989 ) ) ;
#11260 = EDGE_CURVE ( 'NONE', #12048, #2472, #8251, .T. ) ;
#11261 = CARTESIAN_POINT ( 'NONE',  ( 9.153496884233396358, 45.82344744250357849, -9.922878119584453316 ) ) ;
#11262 = DIRECTION ( 'NONE',  ( -0.8660254037844326014, 0.000000000000000000, -0.5000000000000103251 ) ) ;
#11263 = CARTESIAN_POINT ( 'NONE',  ( 11.23155463829053247, 30.71129247825936304, -7.490173329162382210 ) ) ;
#11264 = CIRCLE ( 'NONE', #1641, 26.00000000000000355 ) ;
#11265 = CARTESIAN_POINT ( 'NONE',  ( -5.554567472103006942, 56.47846890177030588, 12.30434293202147167 ) ) ;
#11266 = CARTESIAN_POINT ( 'NONE',  ( -3.811337859253840943, 50.54295824350852939, 12.95086203090105670 ) ) ;
#11267 = CARTESIAN_POINT ( 'NONE',  ( 1.308231877209349081, 32.72703918382474342, 13.43647239758811374 ) ) ;
#11268 = LINE ( 'NONE', #10919, #1200 ) ;
#11269 = CARTESIAN_POINT ( 'NONE',  ( 13.47604474945591058, 39.45782905736723478, -0.8059756131630804177 ) ) ;
#11270 = ORIENTED_EDGE ( 'NONE', *, *, #15700, .F. ) ;
#11271 = CARTESIAN_POINT ( 'NONE',  ( -9.114618562460469420, 62.32545052674210240, 9.962813353323715759 ) ) ;
#11272 = VERTEX_POINT ( 'NONE', #13366 ) ;
#11273 = CARTESIAN_POINT ( 'NONE',  ( 18.62499999999935341, -39.50937499999993463, 7.714727599200469577 ) ) ;
#11274 = CARTESIAN_POINT ( 'NONE',  ( 10.72853415096860275, 48.11889978472238738, 8.194428814822611429 ) ) ;
#11275 = CARTESIAN_POINT ( 'NONE',  ( 0.000000000000000000, 9.000000000000000000, -14.50000000000000000 ) ) ;
#11276 = CARTESIAN_POINT ( 'NONE',  ( 13.50000000000000000, 36.42999999999999972, 1.653273178848926867E-15 ) ) ;
#11277 = CARTESIAN_POINT ( 'NONE',  ( -8.343458848123582072, 40.37999999999998835, 11.48378591275254124 ) ) ;
#11278 = DIRECTION ( 'NONE',  ( 0.000000000000000000, 0.000000000000000000, -1.000000000000000000 ) ) ;
#11279 = CARTESIAN_POINT ( 'NONE',  ( -10.15340906302686719, 67.58731543087333193, -8.897236675027087927 ) ) ;
#11280 = CARTESIAN_POINT ( 'NONE',  ( -4.711679271993003404, 2.046875000000014211, -11.37500000000039613 ) ) ;
#11281 = CARTESIAN_POINT ( 'NONE',  ( 6.729357836367587886, 53.92846635459285665, 11.70346878396139445 ) ) ;
#11282 = VERTEX_POINT ( 'NONE', #1255 ) ;
#11283 = CARTESIAN_POINT ( 'NONE',  ( -0.4537535686862056439, 64.19631530089112914, -13.49237553831279612 ) ) ;
#11284 = ORIENTED_EDGE ( 'NONE', *, *, #4346, .T. ) ;
#11285 = CARTESIAN_POINT ( 'NONE',  ( 8.343458848123580296, 8.980000000000011084, 11.48378591275253768 ) ) ;
#11286 = CARTESIAN_POINT ( 'NONE',  ( -11.34489072193997394, 34.65565179922739247, -7.320614711993081336 ) ) ;
#11287 = CARTESIAN_POINT ( 'NONE',  ( -4.711679271994916540, -44.74687499999989626, 11.37499999999960210 ) ) ;
#11288 = CARTESIAN_POINT ( 'NONE',  ( 13.50002729581672867, 78.43731220364004741, -0.2171257608274307360 ) ) ;
#11289 = CARTESIAN_POINT ( 'NONE',  ( 2.138189944381238661, 46.75688142232026934, 13.50000000000000000 ) ) ;
#11290 = FACE_OUTER_BOUND ( 'NONE', #14597, .T. ) ;
#11291 = CARTESIAN_POINT ( 'NONE',  ( -13.49999999999999822, 37.07999999999999829, 4.386415899144235020 ) ) ;
#11292 = CARTESIAN_POINT ( 'NONE',  ( 13.37264497842671673, 72.36533816201536240, 1.850009941757990717 ) ) ;
#11293 = CARTESIAN_POINT ( 'NONE',  ( -11.76794919243112325, 27.78000000000000114, -3.823638476888998827 ) ) ;
#11294 = CARTESIAN_POINT ( 'NONE',  ( 13.49999999999999822, 66.28000000000001535, 4.386415899144237684 ) ) ;
#11295 = CARTESIAN_POINT ( 'NONE',  ( -1.010931998681471075E-07, 71.67999718330101189, 13.49999999999999822 ) ) ;
#11296 = EDGE_CURVE ( 'NONE', #6427, #14305, #12050, .T. ) ;
#11297 = CARTESIAN_POINT ( 'NONE',  ( -7.272992578804307939, 41.47999999999999687, -10.01041549318726886 ) ) ;
#11298 = CARTESIAN_POINT ( 'NONE',  ( -8.691771469529815392E-16, 58.67999999999998550, 14.19474002721660355 ) ) ;
#11299 = EDGE_CURVE ( 'NONE', #5905, #16027, #13036, .T. ) ;
#11300 = CARTESIAN_POINT ( 'NONE',  ( 1.629909063141895542, 50.73860606154746478, 13.40135283676167965 ) ) ;
#11301 = CARTESIAN_POINT ( 'NONE',  ( -9.520470885617717371, -4.769999999999996021, 6.917026985038133624 ) ) ;
#11302 = CARTESIAN_POINT ( 'NONE',  ( 5.029451273018744395, 68.86152500203888849, 12.52818279675859792 ) ) ;
#11303 = CARTESIAN_POINT ( 'NONE',  ( 1.768248422467277647, 35.74357465886849639, 13.38469673118040504 ) ) ;
#11304 = CARTESIAN_POINT ( 'NONE',  ( 13.16986379959833897, -105.0687499999997527, 13.16986379960055409 ) ) ;
#11305 = CARTESIAN_POINT ( 'NONE',  ( -11.47705729850806122, 73.66444291895690810, -7.108385984861816276 ) ) ;
#11306 = CARTESIAN_POINT ( 'NONE',  ( 0.000000000000000000, 9.999999999999998224, 0.000000000000000000 ) ) ;
#11307 = CARTESIAN_POINT ( 'NONE',  ( 7.416407864998740607, 8.746025403784440044, -10.20780970022447676 ) ) ;
#11308 =( GEOMETRIC_REPRESENTATION_CONTEXT ( 3 ) GLOBAL_UNCERTAINTY_ASSIGNED_CONTEXT ( ( #7343 ) ) GLOBAL_UNIT_ASSIGNED_CONTEXT ( ( #8769, #7609, #1842 ) ) REPRESENTATION_CONTEXT ( 'NONE', 'WORKASPACE' ) );
#11309 = CARTESIAN_POINT ( 'NONE',  ( -4.171729424061791036, 3.530000000000005578, 12.83926296998457239 ) ) ;
#11310 = CARTESIAN_POINT ( 'NONE',  ( -10.92172942406178926, 29.63000000000001677, -7.935100905948389460 ) ) ;
#11311 = CARTESIAN_POINT ( 'NONE',  ( -9.520470885617717371, -4.769999999999996021, 6.917026985038133624 ) ) ;
#11312 = CARTESIAN_POINT ( 'NONE',  ( -7.576616670048093940E-16, 42.67999999999999261, 12.37355403259654807 ) ) ;
#11313 = CARTESIAN_POINT ( 'NONE',  ( 10.92172942406178926, -14.86999999999999389, 7.935100905948385908 ) ) ;
#11314 = CARTESIAN_POINT ( 'NONE',  ( -11.28923155001206347, 32.20771843106157206, 7.402935447327149809 ) ) ;
#11315 = B_SPLINE_CURVE_WITH_KNOTS ( 'NONE', 3,
 ( #4098, #7200, #3204, #1703, #5969, #9865, #3295, #299, #15122, #4547, #13805, #7116, #8709, #12503, #3020, #14069, #16553, #388, #562, #8451, #5794, #7379, #12757, #16641, #1617, #1789, #16463, #8624, #9952, #15216, #13976, #2930, #5709, #11178, #12586, #15388, #4460, #3112, #8361, #1954, #12412, #7033, #15037, #13718, #8540, #645, #4632, #5884, #6055, #13890, #9688, #4278, #475, #1871, #11263, #7287, #11091, #15300, #12670, #11350, #11438, #16725, #9776, #4367, #10038, #13015, #4718, #15473, #896, #8796, #14154, #6486, #2295, #6223, #10120, #2042, #1073, #15731, #3384, #7723, #7466, #16899, #10377, #12846, #3552, #11609, #8883, #4888, #9146, #15642, #735, #6143, #5068, #11522, #16810, #4803, #10205, #15558, #2210, #3469, #3639, #6308, #14238, #2123, #7549, #985, #11693, #12927, #17070, #16985, #812, #10290, #8966, #7815, #14322, #4974, #7638, #9053, #14407, #13099, #6398, #11781, #17157, #14493, #10463, #15823, #3728, #2380, #13188, #10888, #5244, #9489, #10630, #13274, #2556, #9404, #8158, #14835, #15995, #5505, #8248, #16257, #8, #3899, #9317, #13522, #1412 ),
 .UNSPECIFIED., .F., .F.,
 ( 4, 2, 2, 2, 1, 1, 2, 2, 2, 2, 1, 1, 1, 2, 2, 2, 2, 2, 1, 2, 2, 1, 1, 2, 2, 2, 2, 1, 2, 2, 1, 1, 2, 1, 2, 2, 2, 2, 2, 2, 1, 1, 2, 2, 1, 1, 1, 2, 2, 2, 1, 2, 2, 1, 1, 2, 2, 2, 2, 1, 1, 1, 2, 2, 2, 2, 2, 2, 2, 2, 1, 1, 2, 2, 2, 2, 2, 2, 2, 2, 2, 2, 2, 2, 2, 4 ),
 ( 0.9754977937536480903, 0.9755935054967979081, 0.9756413613683727615, 0.9756652893041601882, 0.9756892172399477259, 0.9758806407262472504, 0.9762634876988464105, 0.9770291816440448418, 0.9785605695344414823, 0.9793262634796398025, 0.9795176869659394381, 0.9796133987090892559, 0.9796612545806641092, 0.9796851825164515359, 0.9797091104522390737, 0.9800919574248382338, 0.9808576513700365540, 0.9816233453152349853, 0.9817190570583846920, 0.9817310210262785164, 0.9817429849941722297, 0.9817669129299596564, 0.9818147688015345098, 0.9820061922878341454, 0.9823890392604333055, 0.9831547332056317368, 0.9835375801782308969, 0.9837290036645305324, 0.9837529316003179591, 0.9837768595361053858, 0.9838247154076803502, 0.9839204271508300570, 0.9846861210960283772, 0.9847339769676032306, 0.9847579049033906573, 0.9847818328391780840, 0.9848775445823279018, 0.9850689680686274263, 0.9854518150412265864, 0.9856432385275261110, 0.9857389502706759288, 0.9857868061422507822, 0.9857897971342242105, 0.9857927881261976388, 0.9857987701101444955, 0.9858107340780382088, 0.9858346620138257466, 0.9862175089864250177, 0.9869832029316235600, 0.9877488968768222133, 0.9877967527483971777, 0.9878206806841846044, 0.9878326446520783177, 0.9878446086199720311, 0.9879403203631218489, 0.9881317438494214844, 0.9885145908220207556, 0.9892802847672194089, 0.9896631317398186800, 0.9897588434829684978, 0.9898066993545434622, 0.9898306272903308889, 0.9898425912582246022, 0.9898545552261183156, 0.9900459787124179512, 0.9908116726576166045, 0.9915773666028151467, 0.9917687900891147823, 0.9918645018322646001, 0.9918884297680521378, 0.9919123577038395645, 0.9919602135754144179, 0.9923430605480138000, 0.9938744484384109956, 0.9942572954110103778, 0.9946401423836096489, 0.9954058363288083022, 0.9957886833014075734, 0.9959801067877072089, 0.9961715302740068445, 0.9969372242192054978, 0.9977029181644041511, 0.9978943416507037867, 0.9980857651370034223, 0.9984686121096026934, 1.000000000000000000 ),
 .UNSPECIFIED. ) ;
#11316 = CARTESIAN_POINT ( 'NONE',  ( 5.984812564823209335, 74.89834532313686566, 12.10097681524328195 ) ) ;
#11317 = CARTESIAN_POINT ( 'NONE',  ( 8.343458848123583849, 3.879999999999999893, -11.48378591275253768 ) ) ;
#11318 = CARTESIAN_POINT ( 'NONE',  ( -4.171729424061787483, 84.32999999999999829, -12.83926296998457417 ) ) ;
#11319 = EDGE_CURVE ( 'NONE', #8372, #14612, #15108, .T. ) ;
#11320 = CARTESIAN_POINT ( 'NONE',  ( 9.114567266466451656, 51.82565792604705024, -9.971525571875499594 ) ) ;
#11321 = CARTESIAN_POINT ( 'NONE',  ( 17.32050807568873196, 0.000000000000000000, 10.00000000000008171 ) ) ;
#11322 = DIRECTION ( 'NONE',  ( 0.000000000000000000, -1.000000000000000000, 0.000000000000000000 ) ) ;
#11323 = B_SPLINE_CURVE_WITH_KNOTS ( 'NONE', 3,
 ( #13229, #11995, #2167, #11737, #6532, #6264, #10333, #1204, #13059, #17289, #17114, #3594, #10418, #5113, #15953, #5201, #15687, #1032, #2421, #6442, #14364, #6615, #2511, #3775, #17377, #7773, #7592, #12971, #9101, #11911, #15776, #10591, #9006, #13144, #10507, #5019, #16037, #3687, #3859, #11825, #853, #15868, #11651, #17028, #9188, #4933, #2252, #14453, #9273, #2340, #14536, #7855, #3946, #14626, #7941, #5291, #10673, #236, #16483, #8383, #13483, #4121, #6786, #2775, #7053, #13568, #8027, #13396, #2955, #4032, #14710, #9446, #14794, #17457, #147, #2598, #8296, #12434, #4387, #12165, #13653, #16396, #10936, #2686, #14974, #9535, #16210, #8117, #1460, #5729, #1284, #4210, #10759, #6698, #14879, #1636, #2865, #1371, #57, #11025, #4299, #15055, #5553, #1547, #5460, #9711, #8206, #13738, #16122, #10843, #6966, #6880, #12252, #320, #16303, #9623, #11110, #12345, #5642, #12078, #5371, #7487, #12868, #756, #4652, #7138, #7307, #4480, #8730, #10060, #3223, #14088, #8472, #5816, #1805, #12692, #3405, #8558, #495, #13822, #6165, #11199, #3132, #15410, #7219, #12606, #8819, #5902, #13911, #2062, #4565, #11281, #6078, #16658, #9972, #16575, #580, #15236, #9887, #15319, #8644, #1975, #3316, #13997, #7399, #1723, #1892, #5990, #11373, #14178, #16744, #12780, #12524, #11545, #408, #667, #11459, #16835, #4738, #10143, #15494, #16922, #9798, #15144 ),
 .UNSPECIFIED., .F., .F.,
 ( 4, 2, 2, 2, 1, 1, 1, 2, 2, 1, 2, 1, 1, 1, 2, 2, 2, 2, 2, 1, 1, 1, 2, 2, 2, 2, 1, 1, 2, 2, 1, 2, 2, 2, 2, 1, 1, 1, 1, 1, 1, 1, 2, 2, 1, 2, 2, 2, 2, 1, 2, 2, 1, 1, 2, 2, 2, 2, 1, 2, 2, 2, 2, 2, 2, 2, 1, 1, 2, 2, 2, 2, 2, 2, 2, 2, 2, 2, 2, 2, 1, 1, 1, 2, 2, 2, 1, 1, 1, 2, 2, 2, 1, 1, 2, 2, 1, 2, 2, 2, 2, 1, 1, 1, 1, 1, 1, 2, 2, 2, 2, 2, 4 ),
 ( 0.5049162376868217006, 0.5058378572734049117, 0.5067594768599881228, 0.5069898817566339533, 0.5071050842049568130, 0.5071626854291182429, 0.5071914860411990134, 0.5072058863472392876, 0.5072202866532796728, 0.5076810964465712228, 0.5081419062398627728, 0.5082571086881857436, 0.5083147099123471735, 0.5083435105244278329, 0.5083579108304682181, 0.5083723111365086034, 0.5086027160331543229, 0.5090635258264457619, 0.5092939307230914814, 0.5094091331714143411, 0.5094667343955757710, 0.5094955350076564304, 0.5095099353136968157, 0.5095243356197372009, 0.5104459552063200789, 0.5113675747929029569, 0.5118283845861943959, 0.5119435870345172557, 0.5120011882586786855, 0.5120299888707593450, 0.5120587894828401154, 0.5122891943794857239, 0.5132108139660684909, 0.5132684151902299208, 0.5132972158023106912, 0.5133260164143913507, 0.5134412188627142104, 0.5136716237593599299, 0.5141324335526512579, 0.5143628384492969774, 0.5144780408976198371, 0.5145068415097004966, 0.5145212418157408818, 0.5145284419687611299, 0.5145356421217812670, 0.5145932433459426969, 0.5150540531392339139, 0.5159756727258163478, 0.5168972923123987817, 0.5170124947607216415, 0.5170268950667619157, 0.5170412953728023009, 0.5170700959848829603, 0.5171276972090443902, 0.5173581021056899987, 0.5178189118989813267, 0.5187405314855637606, 0.5192013412788549775, 0.5194317461755006970, 0.5194893473996620159, 0.5195469486238234458, 0.5196621510721463055, 0.5215053902453112844, 0.5219662000386025014, 0.5220238012627639312, 0.5220382015688043165, 0.5220526018748445907, 0.5220814024869253611, 0.5221966049352481098, 0.5224270098318937183, 0.5233486294184762633, 0.5242702490050588082, 0.5245006539017044167, 0.5246158563500272765, 0.5247310587983501362, 0.5251918685916413532, 0.5256526783849325701, 0.5257678808332554299, 0.5257822811392958151, 0.5257894812923159522, 0.5257966814453360893, 0.5258254820574168598, 0.5258830832815782896, 0.5261134881782240091, 0.5270351077648066651, 0.5270927089889680950, 0.5271503102131295249, 0.5272655126614523846, 0.5274959175580981041, 0.5279567273513894321, 0.5288783469379721991, 0.5293391567312635271, 0.5294543591795863868, 0.5295119604037478167, 0.5295407610158285872, 0.5295551613218688614, 0.5295695616279092466, 0.5297999665245549661, 0.5307215861111376221, 0.5307791873352990519, 0.5308367885594604818, 0.5309519910077833416, 0.5311823959044290611, 0.5316432056977203890, 0.5318736105943661086, 0.5319888130426889683, 0.5320176136547696277, 0.5320320139608100130, 0.5320464142668503982, 0.5321040154910118281, 0.5325648252843031560, 0.5334864448708860341, 0.5344080644574688010 ),
 .UNSPECIFIED. ) ;
#11324 = CARTESIAN_POINT ( 'NONE',  ( -22.50000000000000355, -22.00000000000000711, -1.714505518806294835E-15 ) ) ;
#11325 = DIRECTION ( 'NONE',  ( 0.8660254037844363761, 0.000000000000000000, 0.5000000000000041078 ) ) ;
#11326 = CARTESIAN_POINT ( 'NONE',  ( 11.65849161655502542, 63.17672869437035388, 6.808066451784101858 ) ) ;
#11327 = CARTESIAN_POINT ( 'NONE',  ( -11.52888015854957793, 80.93000000000003524, 3.329402692645399675 ) ) ;
#11328 = CARTESIAN_POINT ( 'NONE',  ( 12.26390295534138097, 48.63671511653366508, -5.643290960661551559 ) ) ;
#11329 = CARTESIAN_POINT ( 'NONE',  ( 2.279995255611139653E-15, 24.17999999999999261, -12.37355403259654985 ) ) ;
#11330 = VERTEX_POINT ( 'NONE', #16540 ) ;
#11331 = CARTESIAN_POINT ( 'NONE',  ( 11.76794919243112325, 70.28000000000000114, 3.823638476888997051 ) ) ;
#11332 = CARTESIAN_POINT ( 'NONE',  ( 4.711679271993006957, -22.92812499999992326, 11.37500000000039613 ) ) ;
#11333 = CARTESIAN_POINT ( 'NONE',  ( -4.711679271994915652, -44.74687499999989626, 11.37499999999960210 ) ) ;
#11334 = CARTESIAN_POINT ( 'NONE',  ( 4.171729424061789260, 8.830000000000005400, 12.83926296998457239 ) ) ;
#11335 = EDGE_LOOP ( 'NONE', ( #17228, #13469, #17142, #8385 ) ) ;
#11336 = CARTESIAN_POINT ( 'NONE',  ( -0.4672551503964261221, 43.19680077074366409, -13.49191230240068151 ) ) ;
#11337 = CARTESIAN_POINT ( 'NONE',  ( 3.590940523862469647, 80.93000000000002103, -12.80902731135813255 ) ) ;
#11338 = CARTESIAN_POINT ( 'NONE',  ( 2.621994543952811015E-15, -0.8199999999999973976, -14.19474002721660355 ) ) ;
#11339 = CARTESIAN_POINT ( 'NONE',  ( 1.561832610794586538E-12, -87.41249999999979536, -18.62500000000000000 ) ) ;
#11340 = CARTESIAN_POINT ( 'NONE',  ( 5.739335732908509513, 65.88870427065418767, 12.21924884404352873 ) ) ;
#11341 = CARTESIAN_POINT ( 'NONE',  ( 13.49999999999999822, 81.27999999999998693, 4.386415899144237684 ) ) ;
#11342 = CARTESIAN_POINT ( 'NONE',  ( -9.520470885617717371, 63.23000000000001108, 6.917026985038133624 ) ) ;
#11343 = LINE ( 'NONE', #15381, #2395 ) ;
#11344 = CARTESIAN_POINT ( 'NONE',  ( 3.636496289402157078, 62.03000000000000114, -11.19198476289190936 ) ) ;
#11345 = ADVANCED_FACE ( 'NONE', ( #463 ), #2919, .T. ) ;
#11346 = CARTESIAN_POINT ( 'NONE',  ( -11.22710358024347066, 46.64834459066621264, -7.497684075563164185 ) ) ;
#11347 = CARTESIAN_POINT ( 'NONE',  ( 11.77153775093140453, 45.67521517251212515, -6.609237642556685444 ) ) ;
#11348 = CARTESIAN_POINT ( 'NONE',  ( 0.4427203256037225421, 70.16408690274822391, -13.49318835613360079 ) ) ;
#11349 = AXIS2_PLACEMENT_3D ( 'NONE', #4269, #13879, #13795 ) ;
#11350 = CARTESIAN_POINT ( 'NONE',  ( 11.30690640946770387, 30.70661390184433870, -7.375942793261094366 ) ) ;
#11351 = CARTESIAN_POINT ( 'NONE',  ( -12.81049166330523370, 55.77383991625395510, -4.351154996992983470 ) ) ;
#11352 = CARTESIAN_POINT ( 'NONE',  ( 2.894739436579920166E-06, 50.68008041434205069, 13.49999999999938005 ) ) ;
#11353 = CARTESIAN_POINT ( 'NONE',  ( 13.26911237221029083, 33.34238326213255732, 2.487181046264572259 ) ) ;
#11354 = B_SPLINE_CURVE_WITH_KNOTS ( 'NONE', 3,
 ( #9940, #2742, #11428, #11337, #17060, #13003, #5957, #7366, #11684, #12746, #11599, #8786, #4964, #7539, #14228, #16976, #15548, #3373, #16714, #3460, #547, #4706, #3190, #16799, #14143, #15462, #15632, #802 ),
 .UNSPECIFIED., .F., .F.,
 ( 4, 2, 2, 2, 2, 2, 2, 2, 2, 2, 2, 2, 2, 4 ),
 ( 0.000000000000000000, 0.002887961676758743750, 0.004331942515138114541, 0.005775923353517485766, 0.007219904191896856123, 0.008663885030276227348, 0.01155184670703496633, 0.01299582754541433668, 0.01443980838379370357, 0.01588378922217307393, 0.01732777006055244429, 0.02021573173731117806, 0.02165971257569054842, 0.02310369341406991878 ),
 .UNSPECIFIED. ) ;
#11355 = CARTESIAN_POINT ( 'NONE',  ( 1.227961615663091699, 43.13597886236095746, -13.44709991383356495 ) ) ;
#11356 = CARTESIAN_POINT ( 'NONE',  ( 10.37184659297094846, 39.76092788044618231, -8.641630322754368265 ) ) ;
#11357 = ORIENTED_EDGE ( 'NONE', *, *, #16042, .T. ) ;
#11358 = CARTESIAN_POINT ( 'NONE',  ( -12.78755855970386968, 62.08593128313325593, 4.328318190136370980 ) ) ;
#11359 = ORIENTED_EDGE ( 'NONE', *, *, #3866, .T. ) ;
#11360 = CARTESIAN_POINT ( 'NONE',  ( -13.03040177922608933, 40.80407172380693481, -3.529905272466287602 ) ) ;
#11361 = CARTESIAN_POINT ( 'NONE',  ( 3.636496289402157078, -17.96999999999999886, -11.19198476289190936 ) ) ;
#11362 = CARTESIAN_POINT ( 'NONE',  ( -7.714727599200466912, -85.29687499999984368, 18.62499999999935341 ) ) ;
#11363 = CARTESIAN_POINT ( 'NONE',  ( 11.72395686480903798, 48.18137790691303479, 6.693342665092507637 ) ) ;
#11364 = AXIS2_PLACEMENT_3D ( 'NONE', #12213, #5775, #5420 ) ;
#11365 = CARTESIAN_POINT ( 'NONE',  ( 2.974383071351499819, 58.07333263741331564, -13.17907237816856814 ) ) ;
#11366 = CARTESIAN_POINT ( 'NONE',  ( 13.50000000000000000, 33.42999999999999261, 1.653273178848926867E-15 ) ) ;
#11367 = CARTESIAN_POINT ( 'NONE',  ( 10.92172942406179104, 38.73000000000000398, -7.935100905948385908 ) ) ;
#11368 = CARTESIAN_POINT ( 'NONE',  ( 8.549612433556128696E-08, 65.68000242247177312, 13.49999999999999822 ) ) ;
#11369 = CARTESIAN_POINT ( 'NONE',  ( -0.8552964561740145077, 8.007719221390686926, 18.18372103750109758 ) ) ;
#11370 = FACE_OUTER_BOUND ( 'NONE', #1289, .T. ) ;
#11371 = CARTESIAN_POINT ( 'NONE',  ( 4.711679271993006957, -22.92812499999992326, 11.37500000000039613 ) ) ;
#11372 = VECTOR ( 'NONE', #13894, 1000.000000000000114 ) ;
#11373 = CARTESIAN_POINT ( 'NONE',  ( 3.927706695870254894, 53.82098454782523334, 12.91925010199899404 ) ) ;
#11374 = ORIENTED_EDGE ( 'NONE', *, *, #10545, .T. ) ;
#11375 = CARTESIAN_POINT ( 'NONE',  ( -5.598125747105554773, 64.38316814361185436, -12.28681845237412240 ) ) ;
#11376 = ORIENTED_EDGE ( 'NONE', *, *, #7267, .F. ) ;
#11377 = CARTESIAN_POINT ( 'NONE',  ( 5.253982477109049753, 66.98991576002745774, -12.43579786932437514 ) ) ;
#11378 = CARTESIAN_POINT ( 'NONE',  ( -5.489207653998832370, 34.37901037099156554, -12.33365157413798308 ) ) ;
#11379 = CARTESIAN_POINT ( 'NONE',  ( -11.37500000000039613, -42.66562499999989200, 4.711679271993002516 ) ) ;
#11380 = CARTESIAN_POINT ( 'NONE',  ( 10.30926263822041733, 78.09576994560912055, 8.718911663792482614 ) ) ;
#11381 = CARTESIAN_POINT ( 'NONE',  ( -10.84872848410749668, 7.815608730986070007, -15.50112061769889493 ) ) ;
#11382 = DIRECTION ( 'NONE',  ( 0.000000000000000000, 0.000000000000000000, 1.000000000000000000 ) ) ;
#11383 = CARTESIAN_POINT ( 'NONE',  ( 7.500000000000000888, -25.28130420966589753, 8.086389325435073161 ) ) ;
#11384 = CARTESIAN_POINT ( 'NONE',  ( 11.80346242492321274, 72.67293280733154859, -6.552678632547006998 ) ) ;
#11385 = CARTESIAN_POINT ( 'NONE',  ( -9.520470885617715595, 30.63000000000001677, -6.917026985038136289 ) ) ;
#11386 = CARTESIAN_POINT ( 'NONE',  ( 13.50000000000000355, 63.57999999999999829, -4.386415899144233244 ) ) ;
#11387 = CARTESIAN_POINT ( 'NONE',  ( -6.092287277825001901, 52.40267620124564729, -12.04843092496792778 ) ) ;
#11388 = CIRCLE ( 'NONE', #3756, 6.000000000000000000 ) ;
#11389 = CARTESIAN_POINT ( 'NONE',  ( 11.76794919243112325, 43.28000000000000114, 3.823638476888996607 ) ) ;
#11390 = CARTESIAN_POINT ( 'NONE',  ( 9.520470885617715595, -15.86999999999999567, 6.917026985038135400 ) ) ;
#11391 = CARTESIAN_POINT ( 'NONE',  ( 10.92172942406179104, 59.73000000000000398, -7.935100905948385908 ) ) ;
#11392 = FACE_OUTER_BOUND ( 'NONE', #13109, .T. ) ;
#11393 = CARTESIAN_POINT ( 'NONE',  ( 7.272992578804308828, -7.020000000000005791, 10.01041549318726709 ) ) ;
#11394 = CARTESIAN_POINT ( 'NONE',  ( -4.359978608474780692, 68.52319895195806509, 12.77656657477075619 ) ) ;
#11395 = CARTESIAN_POINT ( 'NONE',  ( 18.62500000000000000, 0.000000000000000000, 1.560692158462880521E-12 ) ) ;
#11396 = FACE_OUTER_BOUND ( 'NONE', #9713, .T. ) ;
#11397 = CARTESIAN_POINT ( 'NONE',  ( 18.62500000000064304, -1.040624999999997469, -7.714727599197335195 ) ) ;
#11398 = CARTESIAN_POINT ( 'NONE',  ( -13.47669604685034273, 73.95737517794891858, 0.7929544294831025741 ) ) ;
#11399 = CARTESIAN_POINT ( 'NONE',  ( -4.681627421645250919, 76.34857381001411625, -12.66224289353729482 ) ) ;
#11400 = DIRECTION ( 'NONE',  ( 0.000000000000000000, 1.000000000000000000, 0.000000000000000000 ) ) ;
#11401 = DIRECTION ( 'NONE',  ( 0.000000000000000000, 1.000000000000000000, 0.000000000000000000 ) ) ;
#11402 = CARTESIAN_POINT ( 'NONE',  ( -7.409984580736203970E-16, -7.320000000000002949, 12.37355403259654985 ) ) ;
#11403 = EDGE_CURVE ( 'NONE', #1796, #15915, #3101, .T. ) ;
#11404 = CARTESIAN_POINT ( 'NONE',  ( -9.520470885617717371, 36.22999999999999687, 6.917026985038133624 ) ) ;
#11405 = UNCERTAINTY_MEASURE_WITH_UNIT (LENGTH_MEASURE( 1.000000000000000082E-05 ), #529, 'distance_accuracy_value', 'NONE');
#11406 = CARTESIAN_POINT ( 'NONE',  ( -12.50000000000000000, 98.93000000000002103, 1.224646799147353059E-15 ) ) ;
#11407 = CARTESIAN_POINT ( 'NONE',  ( -5.430539838780684470, 32.48335489466801818, 12.36597437050387605 ) ) ;
#11408 = CARTESIAN_POINT ( 'NONE',  ( 0.6357631489675421577, 74.70282378747322127, 13.48670659248960391 ) ) ;
#11409 = CARTESIAN_POINT ( 'NONE',  ( 0.000000000000000000, 0.000000000000000000, 0.000000000000000000 ) ) ;
#11410 = DIRECTION ( 'NONE',  ( 0.000000000000000000, 0.000000000000000000, 1.000000000000000000 ) ) ;
#11411 = CARTESIAN_POINT ( 'NONE',  ( -10.92172942406179104, 79.23000000000000398, 7.935100905948387684 ) ) ;
#11412 = CARTESIAN_POINT ( 'NONE',  ( 13.39742027234894373, 51.37205055260678677, 1.661267672429425080 ) ) ;
#11413 = CARTESIAN_POINT ( 'NONE',  ( -3.953315691120589559, 38.53792859346052779, 12.90880018502329740 ) ) ;
#11414 = AXIS2_PLACEMENT_3D ( 'NONE', #11406, #12725, #2259 ) ;
#11415 = CARTESIAN_POINT ( 'NONE',  ( 5.257186988432292374, 36.98950229088148944, -12.43479488390594234 ) ) ;
#11416 = FACE_OUTER_BOUND ( 'NONE', #655, .T. ) ;
#11417 = FACE_OUTER_BOUND ( 'NONE', #3319, .T. ) ;
#11418 = CARTESIAN_POINT ( 'NONE',  ( 11.99276598793104220, 63.20099088703636170, 6.208637428856185636 ) ) ;
#11419 = CARTESIAN_POINT ( 'NONE',  ( 0.7454762885463678268, 41.70680463810530370, 13.47968111932929425 ) ) ;
#11420 = CARTESIAN_POINT ( 'NONE',  ( 13.22392818312517981, 48.52595923520821941, -2.716232255608545199 ) ) ;
#11421 = CARTESIAN_POINT ( 'NONE',  ( 11.76794919243112325, 17.28000000000001535, 3.823638476888996163 ) ) ;
#11422 = ORIENTED_EDGE ( 'NONE', *, *, #7415, .F. ) ;
#11423 = CARTESIAN_POINT ( 'NONE',  ( -3.636496289402153081, 71.32999999999999829, -11.19198476289190936 ) ) ;
#11424 = CARTESIAN_POINT ( 'NONE',  ( -8.043339635996304082, -15.64374999999994387, -8.043339635997652337 ) ) ;
#11425 = CARTESIAN_POINT ( 'NONE',  ( -11.37500000000000000, -58.27499999999986358, -9.545674412382054647E-13 ) ) ;
#11426 = EDGE_CURVE ( 'NONE', #2957, #2562, #7187, .T. ) ;
#11427 = CARTESIAN_POINT ( 'NONE',  ( -1.516382701837864061E-05, 43.18000056530163278, -13.49999999999148237 ) ) ;
#11428 = CARTESIAN_POINT ( 'NONE',  ( 4.992525441478825599, 80.92999999999999261, -12.45192268195328644 ) ) ;
#11429 = CARTESIAN_POINT ( 'NONE',  ( -18.62500000000064659, -42.66562499999989200, 7.714727599197333419 ) ) ;
#11430 = AXIS2_PLACEMENT_3D ( 'NONE', #1295, #6799, #4220 ) ;
#11431 = CARTESIAN_POINT ( 'NONE',  ( 5.638822662700721189, 65.88478960647121596, 12.26611570875842361 ) ) ;
#11432 = DIRECTION ( 'NONE',  ( 0.000000000000000000, 0.000000000000000000, -1.000000000000000000 ) ) ;
#11433 = CARTESIAN_POINT ( 'NONE',  ( 9.520470885617715595, 46.12999999999999545, 6.917026985038134512 ) ) ;
#11434 = CARTESIAN_POINT ( 'NONE',  ( -13.33009014538846060, 46.85508354669458697, -2.135410199497755457 ) ) ;
#11435 = CARTESIAN_POINT ( 'NONE',  ( 13.00530806322553801, 45.55934659475123993, -3.622166112361987711 ) ) ;
#11436 = CARTESIAN_POINT ( 'NONE',  ( 8.581308343826755447, 69.85066467472573493, -10.42246601472090184 ) ) ;
#11437 = LINE ( 'NONE', #4459, #16819 ) ;
#11438 = CARTESIAN_POINT ( 'NONE',  ( 11.32201783469629319, 30.70566325776308148, -7.352740184045440053 ) ) ;
#11439 = CARTESIAN_POINT ( 'NONE',  ( -12.75462880676983346, 56.08956944644259579, 4.424037827898520625 ) ) ;
#11440 = DIRECTION ( 'NONE',  ( -0.000000000000000000, 1.000000000000000000, -0.000000000000000000 ) ) ;
#11441 = CARTESIAN_POINT ( 'NONE',  ( 12.74964865169902595, 33.26969396973853321, 4.447817866060830738 ) ) ;
#11442 = CARTESIAN_POINT ( 'NONE',  ( 0.02127179003657111989, 43.17923766543314912, -13.49998428890246238 ) ) ;
#11443 = CARTESIAN_POINT ( 'NONE',  ( 8.276543950180441200, 39.86464973345010065, -10.66536639688594157 ) ) ;
#11444 = VERTEX_POINT ( 'NONE', #4533 ) ;
#11445 = CARTESIAN_POINT ( 'NONE',  ( -13.47504669145713052, 61.95844030485035603, 0.8236179170182681419 ) ) ;
#11446 = EDGE_LOOP ( 'NONE', ( #998, #16748, #1513, #1808 ) ) ;
#11447 = EDGE_CURVE ( 'NONE', #14369, #16090, #11354, .T. ) ;
#11448 = ORIENTED_EDGE ( 'NONE', *, *, #3771, .F. ) ;
#11449 = CARTESIAN_POINT ( 'NONE',  ( 13.16986379960055409, -92.58124999999979821, -13.16986379959834430 ) ) ;
#11450 = CARTESIAN_POINT ( 'NONE',  ( 11.44020875125550418, 48.16198584060624199, 7.171056752996642025 ) ) ;
#11451 = CARTESIAN_POINT ( 'NONE',  ( 2.429919961663213446, 58.09262903994793703, -13.27951469578883170 ) ) ;
#11452 = CARTESIAN_POINT ( 'NONE',  ( 4.962992231027985923, 79.00097767184028896, -12.55463077525622850 ) ) ;
#11453 = CARTESIAN_POINT ( 'NONE',  ( -3.636496289402153081, 77.32999999999999829, -11.19198476289190936 ) ) ;
#11454 = CARTESIAN_POINT ( 'NONE',  ( -13.49999999999999822, 42.77999999999999403, -4.386415899144240349 ) ) ;
#11455 = CARTESIAN_POINT ( 'NONE',  ( -1.080702808754571365, 46.21883424019694075, -13.45909926978481685 ) ) ;
#11456 = CARTESIAN_POINT ( 'NONE',  ( -0.6268641640632613976, 67.20253659941207047, -13.48655692365852765 ) ) ;
#11457 = CARTESIAN_POINT ( 'NONE',  ( -9.552639591052204498E-13, -38.53749999999988063, 11.37500000000000178 ) ) ;
#11458 = AXIS2_PLACEMENT_3D ( 'NONE', #2461, #6567, #7892 ) ;
#11459 = CARTESIAN_POINT ( 'NONE',  ( 3.249354579472210958, 53.79684832599942723, 13.10312257493411892 ) ) ;
#11460 = ORIENTED_EDGE ( 'NONE', *, *, #3366, .F. ) ;
#11461 = DIRECTION ( 'NONE',  ( 0.000000000000000000, -1.000000000000000000, 0.000000000000000000 ) ) ;
#11462 = ORIENTED_EDGE ( 'NONE', *, *, #7558, .F. ) ;
#11463 = CARTESIAN_POINT ( 'NONE',  ( 2.856314228632829799, 67.07729655047123174, -13.19448560150985550 ) ) ;
#11464 = CARTESIAN_POINT ( 'NONE',  ( -4.429559070322160785, 34.33932522792037645, -12.75305594940425813 ) ) ;
#11465 = CARTESIAN_POINT ( 'NONE',  ( 2.621994543952811015E-15, 17.17999999999999972, -14.19474002721660355 ) ) ;
#11466 = CARTESIAN_POINT ( 'NONE',  ( 4.711679271993006068, -80.12812499999981242, 11.37500000000039257 ) ) ;
#11467 = CARTESIAN_POINT ( 'NONE',  ( 2.224888343446056904, 77.75999185975226169, 13.31734366878287190 ) ) ;
#11468 = CARTESIAN_POINT ( 'NONE',  ( -1.167348460861534098, 59.63805143168455203, 13.45207174649093140 ) ) ;
#11469 = CARTESIAN_POINT ( 'NONE',  ( 15.43323788540791419, 8.055324194567102580, 9.314791131849325723 ) ) ;
#11470 = CARTESIAN_POINT ( 'NONE',  ( -7.499999999999996447, -22.00000000000000000, -9.367496997597603681 ) ) ;
#11471 = CARTESIAN_POINT ( 'NONE',  ( 13.50427256397625442, 72.45803527614656048, -0.8161559238757217782 ) ) ;
#11472 = CARTESIAN_POINT ( 'NONE',  ( 9.520470885617715595, 26.13000000000001322, 6.917026985038135400 ) ) ;
#11473 = AXIS2_PLACEMENT_3D ( 'NONE', #6485, #13014, #6307 ) ;
#11474 = CARTESIAN_POINT ( 'NONE',  ( -8.343458848123582072, 53.37999999999998835, 11.48378591275254124 ) ) ;
#11475 = CARTESIAN_POINT ( 'NONE',  ( -8.818712758598348245, 52.52050123826117556, -10.22156924380393761 ) ) ;
#11476 = CARTESIAN_POINT ( 'NONE',  ( -7.272992578804310604, -16.62000000000000099, 10.01041549318726709 ) ) ;
#11477 = CARTESIAN_POINT ( 'NONE',  ( -10.92172942406178926, 51.62999999999999545, -7.935100905948389460 ) ) ;
#11478 = CARTESIAN_POINT ( 'NONE',  ( -11.00000000000012612, 0.000000000000000000, 15.58845726811980725 ) ) ;
#11479 = EDGE_CURVE ( 'NONE', #201, #3761, #4878, .T. ) ;
#11480 = CARTESIAN_POINT ( 'NONE',  ( -3.636496289402156190, -1.469999999999999085, 11.19198476289190758 ) ) ;
#11481 = CARTESIAN_POINT ( 'NONE',  ( -1.221649949217112674, 68.63608161155467258, 13.44461842710221866 ) ) ;
#11482 = CARTESIAN_POINT ( 'NONE',  ( 7.714727599197338748, -46.82812499999989342, 18.62500000000063949 ) ) ;
#11483 = CARTESIAN_POINT ( 'NONE',  ( 13.50000000000000355, 71.57999999999999829, -4.386415899144233244 ) ) ;
#11484 = CARTESIAN_POINT ( 'NONE',  ( 13.16986379960055054, -35.38124999999991616, -13.16986379959834430 ) ) ;
#11485 = AXIS2_PLACEMENT_3D ( 'NONE', #15363, #9928, #7093 ) ;
#11486 = CARTESIAN_POINT ( 'NONE',  ( -10.26088610336786999, 65.26697153941822194, 8.775667508859029908 ) ) ;
#11487 = DIRECTION ( 'NONE',  ( 0.000000000000000000, 0.000000000000000000, -1.000000000000000000 ) ) ;
#11488 = CARTESIAN_POINT ( 'NONE',  ( 0.000000000000000000, 108.9300000000000068, 0.000000000000000000 ) ) ;
#11489 = CARTESIAN_POINT ( 'NONE',  ( 10.92172942406178926, 28.13000000000001677, 7.935100905948385908 ) ) ;
#11490 = CARTESIAN_POINT ( 'NONE',  ( -7.272992578804307939, 41.48000000000000398, -10.01041549318727064 ) ) ;
#11491 = CARTESIAN_POINT ( 'NONE',  ( -4.020198640976432536, 40.32452907086292271, -12.88802636581765171 ) ) ;
#11492 = CARTESIAN_POINT ( 'NONE',  ( -11.47301210480950573, 32.19583706789580901, 7.115409834509677012 ) ) ;
#11493 = DIRECTION ( 'NONE',  ( 0.000000000000000000, 0.000000000000000000, 1.000000000000000000 ) ) ;
#11494 = CARTESIAN_POINT ( 'NONE',  ( -0.3977526850660704771, 53.66569853454892325, 13.49421918269976572 ) ) ;
#11495 = CARTESIAN_POINT ( 'NONE',  ( -8.343458848123576743, 78.47999999999998977, -11.48378591275254301 ) ) ;
#11496 = CARTESIAN_POINT ( 'NONE',  ( 12.72736902482333932, 51.59255635549924079, -4.502454855677821222 ) ) ;
#11497 = CARTESIAN_POINT ( 'NONE',  ( -12.51208461251463788, 38.11435409805191199, 5.070052519584926642 ) ) ;
#11498 = CARTESIAN_POINT ( 'NONE',  ( 10.20673554080668310, 36.76984911407893719, -8.836287964642385973 ) ) ;
#11499 = CARTESIAN_POINT ( 'NONE',  ( 11.37500000000039435, -50.99062499999987352, -4.711679271993004292 ) ) ;
#11500 = DIRECTION ( 'NONE',  ( 0.8660254037844332675, 0.000000000000000000, 0.5000000000000092149 ) ) ;
#11501 = CARTESIAN_POINT ( 'NONE',  ( 15.58845726811991916, 0.000000000000000000, -10.99999999999996092 ) ) ;
#11502 = CARTESIAN_POINT ( 'NONE',  ( -3.972390705872383965, 80.53716609899321099, 12.90244840476221633 ) ) ;
#11503 = CARTESIAN_POINT ( 'NONE',  ( 5.833048919164877333, 41.89238145366736887, 12.17567392941536397 ) ) ;
#11504 = CARTESIAN_POINT ( 'NONE',  ( 13.49629668835036789, 48.41912274314424991, 0.3168857007667773007 ) ) ;
#11505 = CARTESIAN_POINT ( 'NONE',  ( 11.76794919243112325, 14.42999999999999794, 1.734723475976807094E-15 ) ) ;
#11506 = ORIENTED_EDGE ( 'NONE', *, *, #6522, .F. ) ;
#11507 = CARTESIAN_POINT ( 'NONE',  ( 2.272985001014427393E-15, 68.18000000000000682, -12.37355403259654807 ) ) ;
#11508 = CARTESIAN_POINT ( 'NONE',  ( -11.37500000000000178, -1.074999999999978639, -9.545674412382054647E-13 ) ) ;
#11509 = CARTESIAN_POINT ( 'NONE',  ( 2.138189944381200469, 57.10311857767973720, -13.50000000000001421 ) ) ;
#11510 = CARTESIAN_POINT ( 'NONE',  ( 13.49999999999999822, 0.2799999999999969180, 4.386415899144237684 ) ) ;
#11511 = CARTESIAN_POINT ( 'NONE',  ( -7.272992578804307939, 30.48000000000000398, -10.01041549318726886 ) ) ;
#11512 = CARTESIAN_POINT ( 'NONE',  ( 0.2986627873522048060, 76.16926118795059608, -13.50000000000000355 ) ) ;
#11513 = CARTESIAN_POINT ( 'NONE',  ( 7.714727599200458030, -36.42187499999990763, -18.62499999999935341 ) ) ;
#11514 = CARTESIAN_POINT ( 'NONE',  ( 4.823391606894267269, 65.85361332035319037, 12.61649015956374065 ) ) ;
#11515 = DIRECTION ( 'NONE',  ( 0.000000000000000000, 0.000000000000000000, 1.000000000000000000 ) ) ;
#11516 = CARTESIAN_POINT ( 'NONE',  ( 9.520470885617717371, 49.72999999999999687, -6.917026985038131848 ) ) ;
#11517 = CARTESIAN_POINT ( 'NONE',  ( 13.50000000000000000, 7.429999999999992610, 1.734723475976807094E-15 ) ) ;
#11518 = CARTESIAN_POINT ( 'NONE',  ( -13.09214566475795571, 59.04778350712611257, 3.306315388002783351 ) ) ;
#11519 = CARTESIAN_POINT ( 'NONE',  ( 13.21252823081788641, 45.52825912558844834, -2.779356458002163688 ) ) ;
#11520 = CARTESIAN_POINT ( 'NONE',  ( 2.196737167881437358, 70.10124606214743892, -13.32735827648023985 ) ) ;
#11521 = ADVANCED_FACE ( 'NONE', ( #6044 ), #8874, .T. ) ;
#11522 = CARTESIAN_POINT ( 'NONE',  ( 13.37271033652606178, 30.49610245274473641, -1.890770679655365827 ) ) ;
#11523 = CARTESIAN_POINT ( 'NONE',  ( -13.41558627325511921, 55.87683987596568613, -1.528904511477074069 ) ) ;
#11524 = CARTESIAN_POINT ( 'NONE',  ( -3.880351607964129368, 50.54047666460265731, 12.93032359281371946 ) ) ;
#11525 = DIRECTION ( 'NONE',  ( 0.000000000000000000, 0.000000000000000000, -1.000000000000000000 ) ) ;
#11526 = DIRECTION ( 'NONE',  ( 0.000000000000000000, -1.000000000000000000, 0.000000000000000000 ) ) ;
#11527 = CARTESIAN_POINT ( 'NONE',  ( 13.00990400852149698, 39.55870865720761742, -3.604563544963208521 ) ) ;
#11528 = VERTEX_POINT ( 'NONE', #13964 ) ;
#11529 = CARTESIAN_POINT ( 'NONE',  ( -13.42561672413123119, 61.87950532278058091, -1.455403704591293534 ) ) ;
#11530 = VERTEX_POINT ( 'NONE', #1860 ) ;
#11531 = VERTEX_POINT ( 'NONE', #7274 ) ;
#11532 = CARTESIAN_POINT ( 'NONE',  ( 8.343458848123578520, 29.98000000000001819, 11.48378591275254124 ) ) ;
#11533 = CARTESIAN_POINT ( 'NONE',  ( -18.62500000000064659, -83.21562499999981810, 7.714727599197333419 ) ) ;
#11534 = CARTESIAN_POINT ( 'NONE',  ( 7.608556374808001621, 57.89437078001525094, -11.15259761450094267 ) ) ;
#11535 = CARTESIAN_POINT ( 'NONE',  ( 10.85989957991099963, 78.73358321125698467, -8.019560153188759699 ) ) ;
#11536 = CARTESIAN_POINT ( 'NONE',  ( 11.76794919243112325, 82.43000000000000682, 1.441158131103945434E-15 ) ) ;
#11537 = CARTESIAN_POINT ( 'NONE',  ( -7.272992578804307939, 83.47999999999998977, -10.01041549318726886 ) ) ;
#11538 = DIRECTION ( 'NONE',  ( 0.000000000000000000, 0.000000000000000000, 1.000000000000000000 ) ) ;
#11539 = B_SPLINE_CURVE_WITH_KNOTS ( 'NONE', 3,
 ( #11698, #11613, #6059, #11442, #14326, #2215, #4807, #3473, #5973, #2046, #16989, #11355, #7470, #16729, #13019, #3300, #16815, #4893, #10294, #4636, #10043, #17074, #12850, #10124, #6312, #649, #15477, #8713, #15646, #12761, #4978, #15392, #10381, #7383, #3388, #14073, #1960, #739, #8801, #6402, #10719, #13441, #11785, #17161, #13358, #12040, #10467, #1166, #2560, #6577, #14497, #9236, #5248, #6744, #9322, #7990, #7820, #11958, #1247, #2384, #17249, #15828, #4078, #13, #3732, #11874, #16168, #5162, #16084, #10554, #14756, #13278, #17419, #3992, #6659, #7903, #9150, #5334, #5073, #9408, #15913, #3822, #17337, #2470, #2646, #8077, #1328, #13192, #15999, #12124, #1077, #10806, #5417, #9493, #2299, #14590, #6491, #10634, #7727, #13103, #3904, #14672, #990, #7095, #13615, #8163, #4168, #452, #8427, #11154, #8340, #13867, #1679, #16530, #5862, #11069, #4258, #4437, #1769, #13527, #4344, #8517, #11241, #195, #12479, #365, #1596, #16619, #9753, #4523, #15190, #280, #13780, #12301, #9844, #2910, #7178, #10892, #8253, #15098, #6924, #5770, #1416, #6834, #12210, #16442, #3091, #104, #2823, #5509, #12566, #14840, #2734, #2997, #16261, #16352, #9580, #14931, #1508, #7012, #5600, #10982, #9668, #15018, #13696, #12389, #5689, #16791, #14047, #7530, #2191, #7264, #3180, #13954, #8688, #8946, #10272, #11503, #3531, #15453, #15279, #3451, #10017, #7358, #15623, #11676, #7618, #713, #6124, #12995, #3362, #8866, #15365, #16879, #14304, #12648, #12737, #1935, #625, #15539, #6289, #537, #14218, #6036, #11419, #4697, #5947, #794, #877, #17052 ),
 .UNSPECIFIED., .F., .F.,
 ( 4, 2, 1, 1, 1, 1, 2, 2, 2, 2, 1, 1, 2, 2, 1, 2, 2, 2, 2, 2, 1, 2, 1, 1, 2, 2, 1, 2, 2, 2, 2, 2, 2, 2, 2, 2, 2, 2, 1, 1, 1, 1, 1, 2, 2, 1, 2, 1, 1, 2, 2, 1, 1, 2, 2, 2, 2, 2, 2, 2, 1, 1, 2, 2, 2, 2, 2, 1, 1, 1, 2, 1, 2, 2, 2, 2, 2, 1, 1, 2, 2, 2, 2, 2, 2, 1, 1, 2, 2, 2, 2, 2, 2, 2, 1, 2, 2, 2, 2, 2, 2, 1, 2, 2, 2, 2, 2, 1, 2, 2, 1, 1, 2, 1, 2, 2, 1, 1, 1, 2, 2, 2, 2, 2, 4 ),
 ( 0.7402069710304320926, 0.7402141279982914490, 0.7402212849661509164, 0.7402355989018696292, 0.7402642267733071657, 0.7403214825161822388, 0.7404359940019324959, 0.7406650169734327882, 0.7411230629164335948, 0.7420391548024349859, 0.7421536662881852431, 0.7422109220310603162, 0.7422252359667790289, 0.7422395499024978527, 0.7422681777739353892, 0.7424972007454357925, 0.7429552466884364881, 0.7431842696599368914, 0.7432415254028119644, 0.7432987811456871485, 0.7434132926314372947, 0.7438713385744381013, 0.7441003615459383935, 0.7442148730316886507, 0.7442435009031261872, 0.7442721287745637238, 0.7443293845174387968, 0.7447874304604396034, 0.7457035223464411056, 0.7461615682894418011, 0.7462760797751919473, 0.7463905912609422044, 0.7466196142324426077, 0.7475357061184439988, 0.7479937520614448054, 0.7482227750329450977, 0.7482800307758202818, 0.7483372865186953549, 0.7484517980044455010, 0.7489098439474461966, 0.7491388669189465999, 0.7492533784046967460, 0.7493106341475718191, 0.7493392620190093556, 0.7493535759547281794, 0.7493678898904470032, 0.7502839817764483943, 0.7503412375193234674, 0.7503483944871829348, 0.7503519729711125574, 0.7503555514550422911, 0.7503698653907610039, 0.7503984932621985404, 0.7505130047479487976, 0.7507420277194492009, 0.7512000736624500075, 0.7521161655484517317, 0.7523451885199521350, 0.7523738163913896715, 0.7523881303271084953, 0.7524024442628272080, 0.7524597000057023921, 0.7525742114914525382, 0.7530322574344533448, 0.7539483493204549580, 0.7544063952634557646, 0.7544636510063309487, 0.7545209067492060218, 0.7546354182349561679, 0.7548644412064565712, 0.7553224871494573778, 0.7553797428923325619, 0.7554083707637700984, 0.7554369986352076349, 0.7555515101209577811, 0.7557805330924581844, 0.7562385790354591020, 0.7563530905212092481, 0.7564103462640843212, 0.7564389741355218577, 0.7564676020069595053, 0.7566966249784599086, 0.7585288087504631349, 0.7587578317219635382, 0.7587864595934010747, 0.7588150874648386113, 0.7588723432077136843, 0.7589868546934639415, 0.7594449006364647481, 0.7603609925224663613, 0.7608190384654671679, 0.7610480614369676822, 0.7610766893084052187, 0.7611053171798427552, 0.7611625729227178283, 0.7612770844084680855, 0.7621931762944698097, 0.7631092681804716449, 0.7633382911519720482, 0.7633955468948471212, 0.7634241747662847688, 0.7634528026377223053, 0.7635673141234724515, 0.7640253600664732581, 0.7649414519524749823, 0.7653994978954757888, 0.7656285208669761921, 0.7656857766098513762, 0.7657144044812889128, 0.7657287184170076255, 0.7657430323527264493, 0.7658575438384767065, 0.7667736357244784307, 0.7672316816674793483, 0.7674607046389797516, 0.7674750185746985753, 0.7674893325104173991, 0.7675179603818549356, 0.7675752161247300087, 0.7676897276104802659, 0.7686058194964821011, 0.7690638654394830187, 0.7691783769252332759, 0.7692928884109835330, 0.7695219113824839363 ),
 .UNSPECIFIED. ) ;
#11540 = VECTOR ( 'NONE', #16045, 1000.000000000000000 ) ;
#11541 = EDGE_CURVE ( 'NONE', #1725, #13215, #15956, .T. ) ;
#11542 = CARTESIAN_POINT ( 'NONE',  ( 8.343458848123583849, 41.88000000000000256, -11.48378591275253768 ) ) ;
#11543 = CARTESIAN_POINT ( 'NONE',  ( -8.891200544363830713E-16, 34.67999999999999261, 13.50000000000000000 ) ) ;
#11544 = CARTESIAN_POINT ( 'NONE',  ( 4.711679271993006957, -6.278124999999967315, 11.37500000000039613 ) ) ;
#11545 = CARTESIAN_POINT ( 'NONE',  ( 3.280751270289125721, 53.79795775059116636, 13.09529373139613817 ) ) ;
#11546 = ORIENTED_EDGE ( 'NONE', *, *, #12672, .T. ) ;
#11547 = CARTESIAN_POINT ( 'NONE',  ( 1.653273178848926472E-15, 80.93000000000000682, 13.50000000000000000 ) ) ;
#11548 = VERTEX_POINT ( 'NONE', #633 ) ;
#11549 = CARTESIAN_POINT ( 'NONE',  ( 1.109228931819516317, 67.14015256849161517, -13.46182782856074134 ) ) ;
#11550 = CARTESIAN_POINT ( 'NONE',  ( -4.171729424061787483, 17.33000000000001251, -12.83926296998457417 ) ) ;
#11551 = CARTESIAN_POINT ( 'NONE',  ( 11.37500000000039435, -84.29062499999983515, -4.711679271993004292 ) ) ;
#11552 = CONICAL_SURFACE ( 'NONE', #12671, 14.50000000000000000, 1.308996938995753867 ) ;
#11553 = CARTESIAN_POINT ( 'NONE',  ( -1.516382701837864061E-05, 43.18000056530163278, -13.49999999999148237 ) ) ;
#11554 = CARTESIAN_POINT ( 'NONE',  ( -4.866239539597595254, 59.50453715926928311, 12.60008563178253382 ) ) ;
#11555 = CARTESIAN_POINT ( 'NONE',  ( 15.58845726811984811, 7.773118517290097174, 11.00000000000007283 ) ) ;
#11556 = CARTESIAN_POINT ( 'NONE',  ( 2.755455298081545172E-15, 0.000000000000000000, 22.50000000000000355 ) ) ;
#11557 = CARTESIAN_POINT ( 'NONE',  ( 13.37582773222545462, 72.36614543582099657, 1.826812634724402251 ) ) ;
#11558 = CARTESIAN_POINT ( 'NONE',  ( 3.636496289402154414, 31.82999999999999829, 11.19198476289190758 ) ) ;
#11559 =( BOUNDED_CURVE ( )  B_SPLINE_CURVE ( 2, ( #8246, #1322, #6738, #12117, #2728, #10798, #4072, #9487, #8156 ),
 .UNSPECIFIED., .F., .F. ) 
 B_SPLINE_CURVE_WITH_KNOTS ( ( 3, 2, 2, 2, 3 ),
 ( 0.4406885646056058481, 0.4444444444444444198, 0.4500000000000000111, 0.4555555555555555469, 0.4583333333333333148 ),
 .UNSPECIFIED. ) 
 CURVE ( )  GEOMETRIC_REPRESENTATION_ITEM ( )  RATIONAL_B_SPLINE_CURVE ( ( 0.9785624164268468261, 0.9669113481358797557, 1.000000000000000000, 0.9510565162951535312, 1.000000000000000000, 0.9510565162951535312, 1.000000000000000000, 0.9755282581475770431, 0.9755282581475768211 ) ) 
 REPRESENTATION_ITEM ( '' )  );
#11560 = CARTESIAN_POINT ( 'NONE',  ( 4.171729424061791924, 58.03000000000000114, -12.83926296998457239 ) ) ;
#11561 = CARTESIAN_POINT ( 'NONE',  ( -1.099254190772257944, 52.21949712129632815, -13.46198568913586158 ) ) ;
#11562 = EDGE_CURVE ( 'NONE', #3478, #8302, #3950, .T. ) ;
#11563 = FACE_OUTER_BOUND ( 'NONE', #5778, .T. ) ;
#11564 = AXIS2_PLACEMENT_3D ( 'NONE', #6655, #11870, #12206 ) ;
#11565 = CARTESIAN_POINT ( 'NONE',  ( -18.62499999999934985, -90.53437499999978400, -7.714727599200458918 ) ) ;
#11566 = CARTESIAN_POINT ( 'NONE',  ( -4.375457956215162980, 68.52263673597026639, 12.77127380410037460 ) ) ;
#11567 = CARTESIAN_POINT ( 'NONE',  ( 7.714727599200458030, -36.42187499999990763, -18.62499999999934985 ) ) ;
#11568 = CARTESIAN_POINT ( 'NONE',  ( 13.50000000000000000, 71.43000000000000682, 1.653273178848926867E-15 ) ) ;
#11569 = CARTESIAN_POINT ( 'NONE',  ( -1.564113515457998572E-12, -12.48749999999997051, 18.62500000000000000 ) ) ;
#11570 = CARTESIAN_POINT ( 'NONE',  ( -1.755979736915106670, 65.61690310277927551, 13.38701199797056596 ) ) ;
#11571 = DIRECTION ( 'NONE',  ( -0.000000000000000000, -1.000000000000000000, -0.000000000000000000 ) ) ;
#11572 = DIRECTION ( 'NONE',  ( 0.000000000000000000, 1.000000000000000000, 0.000000000000000000 ) ) ;
#11573 = CARTESIAN_POINT ( 'NONE',  ( -8.343458848123582072, 27.38000000000001322, 11.48378591275254124 ) ) ;
#11574 = EDGE_LOOP ( 'NONE', ( #11593, #5139, #10811, #14937 ) ) ;
#11575 = CARTESIAN_POINT ( 'NONE',  ( 2.272985001014427393E-15, 32.17999999999999972, -12.37355403259654807 ) ) ;
#11576 = CARTESIAN_POINT ( 'NONE',  ( 0.000000000000000000, 88.93000000000000682, 0.000000000000000000 ) ) ;
#11577 = CARTESIAN_POINT ( 'NONE',  ( -2.757875465074077770, 40.27916169625384413, -13.21535913837822918 ) ) ;
#11578 = CARTESIAN_POINT ( 'NONE',  ( -12.73613204840894575, 32.09161058603033467, 4.477490723709251164 ) ) ;
#11579 = CARTESIAN_POINT ( 'NONE',  ( 4.363973203552268920, 74.83691680965836213, 12.79366461543962785 ) ) ;
#11580 = CARTESIAN_POINT ( 'NONE',  ( 10.64851715830567969, 60.11437978181223230, 8.298139595169439886 ) ) ;
#11581 = CARTESIAN_POINT ( 'NONE',  ( 2.445080149700053643E-15, 4.180000000000004157, -13.50000000000000000 ) ) ;
#11582 = DIRECTION ( 'NONE',  ( 1.000000000000000000, 0.000000000000000000, 0.000000000000000000 ) ) ;
#11583 = CARTESIAN_POINT ( 'NONE',  ( 13.49703212424635090, 51.44014129662132717, -0.2960093095830344523 ) ) ;
#11584 = CARTESIAN_POINT ( 'NONE',  ( -10.98823275438732594, 38.22618272328060840, 7.843141453616995662 ) ) ;
#11585 = CARTESIAN_POINT ( 'NONE',  ( 13.02171738018827973, 36.55712068918894886, -3.561963326260443985 ) ) ;
#11586 = CARTESIAN_POINT ( 'NONE',  ( 11.37499999999960210, -39.50937499999993463, 4.711679271994916540 ) ) ;
#11587 = CARTESIAN_POINT ( 'NONE',  ( -13.49999999999999822, 69.78000000000000114, -4.386415899144240349 ) ) ;
#11588 = CARTESIAN_POINT ( 'NONE',  ( -0.4449605378473073247, 77.66411776958061353, 13.50000000002665779 ) ) ;
#11589 = CARTESIAN_POINT ( 'NONE',  ( -7.499999999999993783, -28.00000000000000000, 9.367496997597603681 ) ) ;
#11590 = DIRECTION ( 'NONE',  ( -0.000000000000000000, -1.000000000000000000, -0.000000000000000000 ) ) ;
#11591 = CARTESIAN_POINT ( 'NONE',  ( 12.06997253147024907, 48.65274548705490076, -6.050138844817690931 ) ) ;
#11592 = CARTESIAN_POINT ( 'NONE',  ( 7.272992578804311492, 11.88000000000000966, -10.01041549318726709 ) ) ;
#11593 = ORIENTED_EDGE ( 'NONE', *, *, #5182, .F. ) ;
#11594 = CARTESIAN_POINT ( 'NONE',  ( 11.76794919243112325, 61.27999999999999403, 3.823638476888997051 ) ) ;
#11595 = CARTESIAN_POINT ( 'NONE',  ( 4.711679271994911211, -29.17187499999991118, -11.37499999999960743 ) ) ;
#11596 = DIRECTION ( 'NONE',  ( 1.000000000000000000, 0.000000000000000000, 0.000000000000000000 ) ) ;
#11597 = CARTESIAN_POINT ( 'NONE',  ( 8.343458848123578520, -0.02000000000000811892, 11.48378591275254124 ) ) ;
#11598 = CARTESIAN_POINT ( 'NONE',  ( -11.76794919243112325, 30.78000000000001180, -3.823638476888998827 ) ) ;
#11599 = CARTESIAN_POINT ( 'NONE',  ( -1.218708134003366972, 80.92999999999994998, -12.93996086231559950 ) ) ;
#11600 = EDGE_CURVE ( 'NONE', #9328, #14888, #12819, .T. ) ;
#11601 = CARTESIAN_POINT ( 'NONE',  ( -18.62500000000064659, -59.31562499999985505, 7.714727599197333419 ) ) ;
#11602 = CARTESIAN_POINT ( 'NONE',  ( -13.49999999999999822, 79.78000000000001535, -4.386415899144240349 ) ) ;
#11603 = CARTESIAN_POINT ( 'NONE',  ( -7.576616670048093940E-16, 51.68000000000000682, 12.37355403259654985 ) ) ;
#11604 = CARTESIAN_POINT ( 'NONE',  ( 13.49999999999999822, 7.279999999999993143, 4.386415899144236796 ) ) ;
#11605 = CARTESIAN_POINT ( 'NONE',  ( -13.47788786600996858, 58.90332777413669874, -0.7723891097661439442 ) ) ;
#11606 = CARTESIAN_POINT ( 'NONE',  ( 11.46114320549623322, 45.16339242848184199, 7.133879970484350963 ) ) ;
#11607 = DIRECTION ( 'NONE',  ( 0.000000000000000000, 0.000000000000000000, -1.000000000000000000 ) ) ;
#11608 = CARTESIAN_POINT ( 'NONE',  ( 1.653273178848926472E-15, 30.93000000000001393, 13.50000000000000000 ) ) ;
#11609 = CARTESIAN_POINT ( 'NONE',  ( 13.06885327976965350, 30.55053021910186573, -3.384549578735317699 ) ) ;
#11610 = CARTESIAN_POINT ( 'NONE',  ( -13.26782536342165386, 55.84215906510630134, -2.493279635214634471 ) ) ;
#11611 = CARTESIAN_POINT ( 'NONE',  ( -11.03304771478256718, 50.22344490325513533, 7.779581208127924086 ) ) ;
#11612 = CARTESIAN_POINT ( 'NONE',  ( 3.389914706142906464, 64.05807598113629808, -13.07065644264653237 ) ) ;
#11613 = CARTESIAN_POINT ( 'NONE',  ( 0.003459163312698950409, 43.17987605612985647, -13.50000000389382748 ) ) ;
#11614 = CARTESIAN_POINT ( 'NONE',  ( 13.17317126124304139, 39.53500463294717093, -2.964159239871142937 ) ) ;
#11615 = ORIENTED_EDGE ( 'NONE', *, *, #15163, .T. ) ;
#11616 = CARTESIAN_POINT ( 'NONE',  ( 5.684616793965449943, 0.08402701657420055814, -10.77050272896347494 ) ) ;
#11617 = CARTESIAN_POINT ( 'NONE',  ( -6.997891731511667324, 61.43956589088693221, -11.54533655814920046 ) ) ;
#11618 = ORIENTED_EDGE ( 'NONE', *, *, #5116, .T. ) ;
#11619 = VERTEX_POINT ( 'NONE', #7254 ) ;
#11620 = CARTESIAN_POINT ( 'NONE',  ( -4.171729424061787483, 34.32999999999999829, -12.83926296998457417 ) ) ;
#11621 = CARTESIAN_POINT ( 'NONE',  ( -18.62500000000000000, -98.82499999999978968, -1.562973063126292757E-12 ) ) ;
#11622 = ADVANCED_FACE ( 'NONE', ( #12640 ), #5935, .T. ) ;
#11623 = CARTESIAN_POINT ( 'NONE',  ( 10.27722599705290740, 57.76617510714760328, -8.759151267258511453 ) ) ;
#11624 = CARTESIAN_POINT ( 'NONE',  ( 9.860830236870366861, 78.78814180884941720, -9.230709546527805287 ) ) ;
#11625 = CARTESIAN_POINT ( 'NONE',  ( -11.76794919243112325, 74.78000000000000114, -3.823638476888998827 ) ) ;
#11626 = CARTESIAN_POINT ( 'NONE',  ( 3.636496289402157078, 83.03000000000000114, -11.19198476289190936 ) ) ;
#11627 = CARTESIAN_POINT ( 'NONE',  ( 8.000000000000019540, 5.918584287042170544, -24.73863375370596174 ) ) ;
#11628 = CARTESIAN_POINT ( 'NONE',  ( 2.138189944381242213, 42.10311857767972299, -13.49999999999999822 ) ) ;
#11629 = CARTESIAN_POINT ( 'NONE',  ( 0.000000000000000000, 80.93000000000000682, 0.000000000000000000 ) ) ;
#11630 = CARTESIAN_POINT ( 'NONE',  ( -8.043339635997654113, -53.10624999999986073, 8.043339635996304082 ) ) ;
#11631 = CARTESIAN_POINT ( 'NONE',  ( 7.416407864998740607, 5.746025403784432051, -10.20780970022447676 ) ) ;
#11632 = CARTESIAN_POINT ( 'NONE',  ( 6.796988989821601379, 33.92896228189544416, -11.67543111795051480 ) ) ;
#11633 = ORIENTED_EDGE ( 'NONE', *, *, #3832, .T. ) ;
#11634 = DIRECTION ( 'NONE',  ( -0.000000000000000000, 1.000000000000000000, -0.000000000000000000 ) ) ;
#11635 = ORIENTED_EDGE ( 'NONE', *, *, #12292, .T. ) ;
#11636 = LINE ( 'NONE', #16926, #11188 ) ;
#11637 = CARTESIAN_POINT ( 'NONE',  ( 4.711679271994911211, -10.37187499999999396, -11.37499999999960210 ) ) ;
#11638 = CARTESIAN_POINT ( 'NONE',  ( 3.524474397628260203, 77.80665974831858023, 13.03877614333868351 ) ) ;
#11639 = CARTESIAN_POINT ( 'NONE',  ( -7.174930598646008129, 59.41297086956210194, 11.43548786726982769 ) ) ;
#11640 = DIRECTION ( 'NONE',  ( -7.483177508809139424E-15, 0.000000000000000000, 1.000000000000000000 ) ) ;
#11641 = EDGE_CURVE ( 'NONE', #4826, #9259, #5888, .T. ) ;
#11642 = LINE ( 'NONE', #17105, #8292 ) ;
#11643 = CARTESIAN_POINT ( 'NONE',  ( 9.756437614077082543, 72.06660688249944258, 9.330710072649175402 ) ) ;
#11644 = CARTESIAN_POINT ( 'NONE',  ( 13.49999999999999822, 54.27999999999999403, 4.386415899144237684 ) ) ;
#11645 = CARTESIAN_POINT ( 'NONE',  ( -5.787687467190007595, 71.46940676660642566, 12.19642108145509418 ) ) ;
#11646 = VECTOR ( 'NONE', #7436, 1000.000000000000000 ) ;
#11647 = CARTESIAN_POINT ( 'NONE',  ( 18.00011380242310466, 8.062143945083761309, -0.1786886709310844257 ) ) ;
#11648 = CARTESIAN_POINT ( 'NONE',  ( 13.16986379960055054, -52.03124999999987921, -13.16986379959834430 ) ) ;
#11649 = CARTESIAN_POINT ( 'NONE',  ( 2.582823892810359290, 68.77289463184231977, 13.25273780715061456 ) ) ;
#11650 = CARTESIAN_POINT ( 'NONE',  ( 18.62500000000000000, -66.59999999999983800, 1.560692158462880521E-12 ) ) ;
#11651 = CARTESIAN_POINT ( 'NONE',  ( 8.971056075657596551, 54.83247871843056487, -10.09135430922370347 ) ) ;
#11652 = CARTESIAN_POINT ( 'NONE',  ( 7.714727599200458030, -53.07187499999987068, -18.62499999999934985 ) ) ;
#11653 = CARTESIAN_POINT ( 'NONE',  ( -9.725010589135534289, 65.29500619405467887, 9.363680539315007323 ) ) ;
#11654 = CARTESIAN_POINT ( 'NONE',  ( -12.50000000000000000, 98.93000000000002103, 9.000000000000000000 ) ) ;
#11655 = CARTESIAN_POINT ( 'NONE',  ( -7.020346476131678060, 35.41948706349571552, 11.53104520956814305 ) ) ;
#11656 = CARTESIAN_POINT ( 'NONE',  ( 4.171729424061789260, 24.83000000000001961, 12.83926296998457239 ) ) ;
#11657 = ORIENTED_EDGE ( 'NONE', *, *, #498, .F. ) ;
#11658 = CARTESIAN_POINT ( 'NONE',  ( -8.343458848123578520, 8.480000000000000426, -11.48378591275254124 ) ) ;
#11659 =( BOUNDED_CURVE ( )  B_SPLINE_CURVE ( 2, ( #12020, #17400, #5315, #5488, #4239, #11051, #83, #14909, #5753, #1752, #15173, #8324, #13678 ),
 .UNSPECIFIED., .F., .F. ) 
 B_SPLINE_CURVE_WITH_KNOTS ( ( 3, 2, 2, 2, 2, 2, 3 ),
 ( 0.5235885359481271539, 0.5264187442505494641, 0.5320791608553940844, 0.5377395774602385936, 0.5433999940650832139, 0.5490604106699278342, 0.5518906191050926280 ),
 .UNSPECIFIED. ) 
 CURVE ( )  GEOMETRIC_REPRESENTATION_ITEM ( )  RATIONAL_B_SPLINE_CURVE ( ( 0.9755282581475768211, 0.9755282581475772652, 1.000000000000000000, 0.9510565162951535312, 1.000000000000000000, 0.9510565162951535312, 1.000000000000000000, 0.9510565162951535312, 1.000000000000000000, 0.9510565162951535312, 1.000000000000000000, 0.9755282569998020570, 0.9755282581475768211 ) ) 
 REPRESENTATION_ITEM ( '' )  );
#11660 = ADVANCED_FACE ( 'NONE', ( #11748 ), #14374, .F. ) ;
#11661 = CARTESIAN_POINT ( 'NONE',  ( -11.83717302900882551, 31.68955936364634951, -6.490870104775230409 ) ) ;
#11662 = CARTESIAN_POINT ( 'NONE',  ( 0.000000000000000000, 80.93000000000000682, 0.000000000000000000 ) ) ;
#11663 = CARTESIAN_POINT ( 'NONE',  ( 13.49992669839407178, 60.43171412446871216, -0.05011807936940589070 ) ) ;
#11664 = CARTESIAN_POINT ( 'NONE',  ( 4.171729424061789260, -2.169999999999998153, 12.83926296998457239 ) ) ;
#11665 = CARTESIAN_POINT ( 'NONE',  ( 10.92172942406179104, 62.73000000000001108, -7.935100905948385908 ) ) ;
#11666 = CARTESIAN_POINT ( 'NONE',  ( 2.272985001014427788E-15, 56.17999999999999972, -12.37355403259654985 ) ) ;
#11667 = SHAPE_REPRESENTATION_RELATIONSHIP ( 'NONE' , 'NONE' ,  #4322, #11777 ) ;
#11668 = CARTESIAN_POINT ( 'NONE',  ( -4.171729424061791036, 73.53000000000000114, 12.83926296998457239 ) ) ;
#11669 = CARTESIAN_POINT ( 'NONE',  ( 13.24054410806451720, 51.52295701284848661, -2.634018347425864714 ) ) ;
#11670 = CARTESIAN_POINT ( 'NONE',  ( -13.41433228084396312, 37.98342063485497277, 1.534182904327553443 ) ) ;
#11671 = CARTESIAN_POINT ( 'NONE',  ( 13.41223885496773427, 36.48523552608328657, -1.585925835905837689 ) ) ;
#11672 = CARTESIAN_POINT ( 'NONE',  ( -11.37499999999999645, -65.52499999999986358, -9.545674412382054647E-13 ) ) ;
#11673 = CARTESIAN_POINT ( 'NONE',  ( -3.493226371046825651, 74.55439642829867353, 13.04022828054566041 ) ) ;
#11674 = CARTESIAN_POINT ( 'NONE',  ( -11.60036162406280980, 77.18758477582102273, 6.922111537354720845 ) ) ;
#11675 = CARTESIAN_POINT ( 'NONE',  ( 0.2536749733826671460, 62.68912121125626413, 13.49762152966559903 ) ) ;
#11676 = CARTESIAN_POINT ( 'NONE',  ( 5.430970834852819173, 41.87677223918051084, 12.35939327805447263 ) ) ;
#11677 = ORIENTED_EDGE ( 'NONE', *, *, #7816, .T. ) ;
#11678 = CARTESIAN_POINT ( 'NONE',  ( 9.520470885617715595, 17.13000000000000611, 6.917026985038135400 ) ) ;
#11679 = EDGE_LOOP ( 'NONE', ( #16794, #5734, #5099, #9156 ) ) ;
#11680 = CARTESIAN_POINT ( 'NONE',  ( 7.272992578804311492, 61.87999999999999545, -10.01041549318726886 ) ) ;
#11681 = CARTESIAN_POINT ( 'NONE',  ( 11.37499999999960565, -91.60937499999975842, 4.711679271994918317 ) ) ;
#11682 = CARTESIAN_POINT ( 'NONE',  ( 8.000000000000021316, 6.548282979925672542, -22.26874168100114559 ) ) ;
#11683 = CARTESIAN_POINT ( 'NONE',  ( -4.171729424061791036, -3.469999999999993978, 12.83926296998457239 ) ) ;
#11684 = CARTESIAN_POINT ( 'NONE',  ( 0.2248552520821813783, 80.93000000000000682, -13.08843060417381210 ) ) ;
#11685 = CARTESIAN_POINT ( 'NONE',  ( -18.62500000000000000, -41.62499999999990052, -1.562973063126292555E-12 ) ) ;
#11686 = CARTESIAN_POINT ( 'NONE',  ( 4.171729424061789260, 80.82999999999999829, 12.83926296998457417 ) ) ;
#11687 = CARTESIAN_POINT ( 'NONE',  ( -7.576616670048093940E-16, 48.67999999999999261, 12.37355403259654985 ) ) ;
#11688 = CARTESIAN_POINT ( 'NONE',  ( 7.500000000000000888, -21.99999999999990052, -9.367496997597653419 ) ) ;
#11689 = CARTESIAN_POINT ( 'NONE',  ( -13.21743544613662813, 59.02708992862847737, 2.747696697556875733 ) ) ;
#11690 = CARTESIAN_POINT ( 'NONE',  ( 10.40464366657246487, 45.10088306759819687, 8.601957922238709031 ) ) ;
#11691 = CARTESIAN_POINT ( 'NONE',  ( 13.37950080006454989, 69.36708149302486959, 1.803377588645109775 ) ) ;
#11692 = CARTESIAN_POINT ( 'NONE',  ( -2.875760791593931984E-14, 76.17999999999999261, -13.50000000000000000 ) ) ;
#11693 = CARTESIAN_POINT ( 'NONE',  ( 13.50382142429054255, 30.41741325757080716, 0.3602961522248570025 ) ) ;
#11694 = EDGE_CURVE ( 'NONE', #5098, #4526, #10506, .T. ) ;
#11695 = CARTESIAN_POINT ( 'NONE',  ( -8.561537994842248978, 55.50809341652116302, -10.44924880110730392 ) ) ;
#11696 = CARTESIAN_POINT ( 'NONE',  ( -9.186396683897722681, 50.32198487252506425, 9.897154769051333290 ) ) ;
#11697 = FACE_OUTER_BOUND ( 'NONE', #3912, .T. ) ;
#11698 = CARTESIAN_POINT ( 'NONE',  ( -1.516382701837864061E-05, 43.18000056530163278, -13.49999999999148237 ) ) ;
#11699 = CARTESIAN_POINT ( 'NONE',  ( 7.311509977803601679, 38.95289584714333841, 11.35082926183423702 ) ) ;
#11700 = ORIENTED_EDGE ( 'NONE', *, *, #14287, .T. ) ;
#11701 = CARTESIAN_POINT ( 'NONE',  ( -12.30392646493007014, 61.72675570561128211, -5.559945461151370338 ) ) ;
#11702 = CARTESIAN_POINT ( 'NONE',  ( 11.76794919243112680, 8.579999999999994742, -3.823638476888993942 ) ) ;
#11703 = ORIENTED_EDGE ( 'NONE', *, *, #12169, .T. ) ;
#11704 = CARTESIAN_POINT ( 'NONE',  ( -8.194307551003054968, 40.49162043279464029, -10.72866187828134876 ) ) ;
#11705 = ORIENTED_EDGE ( 'NONE', *, *, #7092, .T. ) ;
#11706 = CARTESIAN_POINT ( 'NONE',  ( -8.343458848123582072, 32.38000000000000966, 11.48378591275254124 ) ) ;
#11707 = CARTESIAN_POINT ( 'NONE',  ( -7.714727599200466912, -101.9468749999998067, 18.62499999999935341 ) ) ;
#11708 = CARTESIAN_POINT ( 'NONE',  ( 4.973974161897672275, 47.85944346994435961, 12.55031192319891531 ) ) ;
#11709 = CARTESIAN_POINT ( 'NONE',  ( 1.102885466463079389, 58.14037304227331049, -13.46176891591130698 ) ) ;
#11710 = CARTESIAN_POINT ( 'NONE',  ( 10.15633907889109544, 78.77269066048498303, -8.904669665069901541 ) ) ;
#11711 = CARTESIAN_POINT ( 'NONE',  ( 11.76794919243112325, 76.28000000000000114, 3.823638476888996607 ) ) ;
#11712 = CARTESIAN_POINT ( 'NONE',  ( -8.691771469529815392E-16, 37.67999999999999261, 14.19474002721660355 ) ) ;
#11713 = CARTESIAN_POINT ( 'NONE',  ( 9.520470885617715595, 82.13000000000000966, 6.917026985038134512 ) ) ;
#11714 = DIRECTION ( 'NONE',  ( 0.000000000000000000, 0.000000000000000000, -1.000000000000000000 ) ) ;
#11715 = AXIS2_PLACEMENT_3D ( 'NONE', #10341, #6362, #3434 ) ;
#11716 = EDGE_CURVE ( 'NONE', #15567, #19, #14439, .T. ) ;
#11717 = CARTESIAN_POINT ( 'NONE',  ( 0.000000000000000000, 80.93000000000000682, 0.000000000000000000 ) ) ;
#11718 = CARTESIAN_POINT ( 'NONE',  ( 8.043339635997652337, -28.13124999999991260, -8.043339635996304082 ) ) ;
#11719 = DIRECTION ( 'NONE',  ( -1.000000000000000000, -1.734723475976807094E-16, -0.000000000000000000 ) ) ;
#11720 = CARTESIAN_POINT ( 'NONE',  ( 5.975311483674380142, 33.96202926739386641, -12.10592502158520922 ) ) ;
#11721 = CARTESIAN_POINT ( 'NONE',  ( -13.35309327176764604, 73.86044722355309489, -1.986183259433068615 ) ) ;
#11722 = ORIENTED_EDGE ( 'NONE', *, *, #12269, .T. ) ;
#11723 = CARTESIAN_POINT ( 'NONE',  ( -7.499999999999999112, 102.9300000000000068, 9.367496997597601904 ) ) ;
#11724 = ORIENTED_EDGE ( 'NONE', *, *, #6562, .T. ) ;
#11725 = CARTESIAN_POINT ( 'NONE',  ( 4.711679271993006957, -37.42812499999992326, 11.37500000000039257 ) ) ;
#11726 = DIRECTION ( 'NONE',  ( 0.000000000000000000, 1.000000000000000000, 0.000000000000000000 ) ) ;
#11727 = CARTESIAN_POINT ( 'NONE',  ( -7.230983158322074722, 59.41059414015147411, 11.40016698628919123 ) ) ;
#11728 = DIRECTION ( 'NONE',  ( -1.000000000000000000, -8.673617379884035472E-17, 0.000000000000000000 ) ) ;
#11729 = CARTESIAN_POINT ( 'NONE',  ( -8.343458848123578520, 5.480000000000007532, -11.48378591275254124 ) ) ;
#11730 = CARTESIAN_POINT ( 'NONE',  ( 13.50000000000000355, 51.57999999999999829, -4.386415899144233244 ) ) ;
#11731 = CARTESIAN_POINT ( 'NONE',  ( -3.039585127116079200, 71.57070844762461093, 13.15361936645533092 ) ) ;
#11732 = CARTESIAN_POINT ( 'NONE',  ( 18.46710335681945025, 7.924935997292879897, 1.296119813004090515 ) ) ;
#11733 = CARTESIAN_POINT ( 'NONE',  ( 18.62500000000000000, 7.250000000000001776, 1.560692158462880521E-12 ) ) ;
#11734 = CARTESIAN_POINT ( 'NONE',  ( -3.962338278797073343, 68.53759793175959203, 12.90602271434200077 ) ) ;
#11735 = CARTESIAN_POINT ( 'NONE',  ( -13.16986379959834252, -56.19374999999985931, -13.16986379960055054 ) ) ;
#11736 = EDGE_CURVE ( 'NONE', #14868, #9538, #16048, .T. ) ;
#11737 = CARTESIAN_POINT ( 'NONE',  ( 2.065461445335230017, 55.10580354823416371, -13.34947176806445590 ) ) ;
#11738 = CARTESIAN_POINT ( 'NONE',  ( -1.564113515457998572E-12, -29.13749999999993179, 18.62500000000000000 ) ) ;
#11739 = CARTESIAN_POINT ( 'NONE',  ( -7.603109958011293301, 65.39459751660324116, 11.15547822810680856 ) ) ;
#11740 = LINE ( 'NONE', #3512, #2792 ) ;
#11741 = CARTESIAN_POINT ( 'NONE',  ( -9.443773158109223687, 35.30916239436312054, 9.647063514268658935 ) ) ;
#11742 = ORIENTED_EDGE ( 'NONE', *, *, #6336, .T. ) ;
#11743 = CARTESIAN_POINT ( 'NONE',  ( 8.050216715958701030, 31.03187307936175188, 8.940658242654157206 ) ) ;
#11744 = VECTOR ( 'NONE', #12461, 1000.000000000000000 ) ;
#11745 = CARTESIAN_POINT ( 'NONE',  ( 1.900613283899841299, 4.890856018536052119, 11.99999999999824496 ) ) ;
#11746 = CARTESIAN_POINT ( 'NONE',  ( -2.405887066621936299, 40.26649426164142653, -13.28772887298001848 ) ) ;
#11747 = CARTESIAN_POINT ( 'NONE',  ( -13.08398228043214218, 31.81151393346248213, -3.329647435564872193 ) ) ;
#11748 = FACE_OUTER_BOUND ( 'NONE', #10764, .T. ) ;
#11749 = CARTESIAN_POINT ( 'NONE',  ( 13.05092373128589678, 60.30692759104906742, 3.453064110984449098 ) ) ;
#11750 = CARTESIAN_POINT ( 'NONE',  ( 4.171729424061791924, -9.969999999999998863, -12.83926296998457239 ) ) ;
#11751 = CARTESIAN_POINT ( 'NONE',  ( -7.552751977303077346, 53.39683216713059011, 11.19100968736766255 ) ) ;
#11752 = CARTESIAN_POINT ( 'NONE',  ( 11.76794919243112325, 55.27999999999998693, 3.823638476888996607 ) ) ;
#11753 = CARTESIAN_POINT ( 'NONE',  ( -13.49999999999999822, 76.07999999999999829, 4.386415899144235908 ) ) ;
#11754 = CARTESIAN_POINT ( 'NONE',  ( 12.24683778235814735, 51.63890018789970782, -5.702013043655419722 ) ) ;
#11755 = AXIS2_PLACEMENT_3D ( 'NONE', #12627, #5924, #13844 ) ;
#11756 = CARTESIAN_POINT ( 'NONE',  ( -13.18940372997155563, 38.03370036661469555, 2.928436094923779986 ) ) ;
#11757 = CARTESIAN_POINT ( 'NONE',  ( 9.040794826975059095, 36.82921390846524901, -10.03951093010358697 ) ) ;
#11758 = CARTESIAN_POINT ( 'NONE',  ( 8.043339635997652337, -75.93124999999983515, -8.043339635996302306 ) ) ;
#11759 = CARTESIAN_POINT ( 'NONE',  ( -0.6196373872324472121, 74.65772012599740037, 13.48577371833401095 ) ) ;
#11760 =( BOUNDED_CURVE ( )  B_SPLINE_CURVE ( 2, ( #1351, #7119, #4281, #6767, #7037, #12145, #12415, #35, #4101, #13637, #9517, #218, #5624 ),
 .UNSPECIFIED., .F., .F. ) 
 B_SPLINE_CURVE_WITH_KNOTS ( ( 3, 2, 2, 2, 2, 2, 3 ),
 ( 0.5138888888888888395, 0.5166666666666667185, 0.5222222222222222543, 0.5277777777777777901, 0.5333333333333333259, 0.5388888888888888618, 0.5416666666666666297 ),
 .UNSPECIFIED. ) 
 CURVE ( )  GEOMETRIC_REPRESENTATION_ITEM ( )  RATIONAL_B_SPLINE_CURVE ( ( 0.9755282581475768211, 0.9755282581475762660, 1.000000000000000000, 0.9510565162951535312, 1.000000000000000000, 0.9510565162951535312, 1.000000000000000000, 0.9510565162951535312, 1.000000000000000000, 0.9510565162951535312, 1.000000000000000000, 0.9755282581475768211, 0.9755282581475768211 ) ) 
 REPRESENTATION_ITEM ( '' )  );
#11761 = CARTESIAN_POINT ( 'NONE',  ( -12.00653703015586515, 77.15764966734894870, 6.172573912317796285 ) ) ;
#11762 = CARTESIAN_POINT ( 'NONE',  ( -8.343458848123582072, 61.38000000000000256, 11.48378591275253768 ) ) ;
#11763 = CARTESIAN_POINT ( 'NONE',  ( 7.500000000000000000, -7.999999999999998224, -22.50000000000000355 ) ) ;
#11764 = ORIENTED_EDGE ( 'NONE', *, *, #5501, .F. ) ;
#11765 = CARTESIAN_POINT ( 'NONE',  ( -7.272992578804307939, 9.480000000000009308, -10.01041549318726886 ) ) ;
#11766 = ORIENTED_EDGE ( 'NONE', *, *, #8596, .T. ) ;
#11767 = CARTESIAN_POINT ( 'NONE',  ( 11.76794919243112680, 61.57999999999999829, -3.823638476888993942 ) ) ;
#11768 = CARTESIAN_POINT ( 'NONE',  ( 9.538709233711902776E-13, -46.86249999999987637, -11.37500000000000178 ) ) ;
#11769 = CARTESIAN_POINT ( 'NONE',  ( -4.711679271994915652, -94.69687499999976410, 11.37499999999960210 ) ) ;
#11770 = CARTESIAN_POINT ( 'NONE',  ( 7.895834936963976425, 75.88172377336412922, -10.95133422968197578 ) ) ;
#11771 = VECTOR ( 'NONE', #7663, 1000.000000000000000 ) ;
#11772 = CARTESIAN_POINT ( 'NONE',  ( 2.138189944381242213, 33.10311857767972299, -13.49999999999999822 ) ) ;
#11773 = CARTESIAN_POINT ( 'NONE',  ( -13.49999999999999822, 68.07999999999998408, 4.386415899144235908 ) ) ;
#11774 = CARTESIAN_POINT ( 'NONE',  ( -11.76794919243112325, 38.92999999999999972, -2.882316262207890869E-15 ) ) ;
#11775 = LINE ( 'NONE', #17151, #7515 ) ;
#11776 = CARTESIAN_POINT ( 'NONE',  ( -11.05161298094616384, 59.22233715161402756, 7.753204029402317232 ) ) ;
#11777 = ADVANCED_BREP_SHAPE_REPRESENTATION ( '', ( #3202, #16654 ), #7660 ) ;
#11778 = CARTESIAN_POINT ( 'NONE',  ( 9.435697569393814987, 45.05040745589252538, 9.656000601265819938 ) ) ;
#11779 = CARTESIAN_POINT ( 'NONE',  ( 13.10046565438790900, 69.54592110386441561, -3.260037864952345377 ) ) ;
#11780 = CARTESIAN_POINT ( 'NONE',  ( 2.452460625982255227, 80.76816317512970045, 13.29106717814962835 ) ) ;
#11781 = CARTESIAN_POINT ( 'NONE',  ( 12.75594003600799908, 30.26868555994605359, 4.481693421996284954 ) ) ;
#11782 = CARTESIAN_POINT ( 'NONE',  ( -4.048254027269543087, 55.32555987908665429, -12.87879573082893714 ) ) ;
#11783 = CARTESIAN_POINT ( 'NONE',  ( -5.602506701022878843, 50.47661089226183151, 12.28261366399036980 ) ) ;
#11784 = CARTESIAN_POINT ( 'NONE',  ( 5.344403403599800484, 63.98653430214261562, -12.39707219021102347 ) ) ;
#11785 = CARTESIAN_POINT ( 'NONE',  ( 5.813490055168404780, 42.96841201847881564, -12.18495851764158111 ) ) ;
#11786 = CARTESIAN_POINT ( 'NONE',  ( 12.95529851766885265, 39.29347969363125515, 3.812543400925126669 ) ) ;
#11787 = EDGE_LOOP ( 'NONE', ( #7220, #12607, #10020, #8803 ) ) ;
#11788 = CARTESIAN_POINT ( 'NONE',  ( 1.653273178848926472E-15, 80.93000000000000682, 13.50000000000000000 ) ) ;
#11789 = CARTESIAN_POINT ( 'NONE',  ( -5.360921580443687162, 70.37408821014601301, -12.39000541084428875 ) ) ;
#11790 = CARTESIAN_POINT ( 'NONE',  ( -11.53742970777352106, 61.66777873792855758, -7.029701866567251933 ) ) ;
#11791 = CARTESIAN_POINT ( 'NONE',  ( 3.636496289402157078, 3.030000000000004690, -11.19198476289190936 ) ) ;
#11792 = EDGE_LOOP ( 'NONE', ( #11270, #17187, #5716, #10597 ) ) ;
#11793 = CARTESIAN_POINT ( 'NONE',  ( -8.101227806547106169, 40.48742319736930995, -10.79914935875280868 ) ) ;
#11794 = VERTEX_POINT ( 'NONE', #2522 ) ;
#11795 = CARTESIAN_POINT ( 'NONE',  ( 13.50000000000000000, 24.43000000000000682, 1.734723475976807094E-15 ) ) ;
#11796 = CARTESIAN_POINT ( 'NONE',  ( -18.62500000000000000, -91.57499999999977547, -1.562973063126292555E-12 ) ) ;
#11797 = CARTESIAN_POINT ( 'NONE',  ( 5.060896339973242064, 47.86270747902148059, 12.51549536631464754 ) ) ;
#11798 = CARTESIAN_POINT ( 'NONE',  ( 12.77833647190731092, 57.27053577403307827, 4.428673400738554200 ) ) ;
#11799 = CARTESIAN_POINT ( 'NONE',  ( 12.15329104187025955, 78.64596498996522200, -5.877850047516828269 ) ) ;
#11800 = ADVANCED_FACE ( 'NONE', ( #13240 ), #15964, .T. ) ;
#11801 = CARTESIAN_POINT ( 'NONE',  ( -11.76794919243112325, 77.92999999999999261, -2.882316262207890869E-15 ) ) ;
#11802 = CARTESIAN_POINT ( 'NONE',  ( -11.76794919243112325, 74.78000000000000114, -3.823638476888998827 ) ) ;
#11803 = CARTESIAN_POINT ( 'NONE',  ( 0.000000000000000000, 9.000000000000000000, 0.000000000000000000 ) ) ;
#11804 = CARTESIAN_POINT ( 'NONE',  ( 0.000000000000000000, 75.00000000000000000, 5.000000000000000000 ) ) ;
#11805 = CARTESIAN_POINT ( 'NONE',  ( -4.711679271993003404, -81.20312499999978684, -11.37500000000039613 ) ) ;
#11806 = CARTESIAN_POINT ( 'NONE',  ( 2.445080149700053643E-15, 63.17999999999998550, -13.50000000000000000 ) ) ;
#11807 = FACE_OUTER_BOUND ( 'NONE', #12347, .T. ) ;
#11808 = B_SPLINE_CURVE_WITH_KNOTS ( 'NONE', 3,
 ( #4546, #15387, #734, #9951, #9775, #4717, #15215, #8450, #12756, #10119 ),
 .UNSPECIFIED., .F., .F.,
 ( 4, 2, 2, 2, 4 ),
 ( 2.344023999656933974E-07, 0.0005276420589627336087, 0.001055049715525501657, 0.001582457372088269705, 0.002109865028651037970 ),
 .UNSPECIFIED. ) ;
#11809 = CARTESIAN_POINT ( 'NONE',  ( -13.37510790282587081, 73.86589262026581082, -1.834146428142618301 ) ) ;
#11810 = EDGE_LOOP ( 'NONE', ( #7827, #11700, #1638, #3845 ) ) ;
#11811 = VERTEX_POINT ( 'NONE', #12003 ) ;
#11812 = CARTESIAN_POINT ( 'NONE',  ( 0.000000000000000000, 30.93000000000001393, 0.000000000000000000 ) ) ;
#11813 = ORIENTED_EDGE ( 'NONE', *, *, #5035, .F. ) ;
#11814 = CARTESIAN_POINT ( 'NONE',  ( 2.621994543952811015E-15, 13.17999999999999616, -14.19474002721660355 ) ) ;
#11815 = CARTESIAN_POINT ( 'NONE',  ( 7.272992578804311492, -12.12000000000000455, -10.01041549318726709 ) ) ;
#11816 = CARTESIAN_POINT ( 'NONE',  ( -9.552639591052204498E-13, -19.73749999999997229, 11.37499999999999645 ) ) ;
#11817 = CARTESIAN_POINT ( 'NONE',  ( -5.930465559976500600, 44.46394333671532451, 12.13728569908712451 ) ) ;
#11818 = CARTESIAN_POINT ( 'NONE',  ( 10.00000000000002132, 0.000000000000000000, -17.32050807568876394 ) ) ;
#11819 = CARTESIAN_POINT ( 'NONE',  ( 9.909898397854359331, 66.78548077375248226, -9.167550852036580267 ) ) ;
#11820 = CARTESIAN_POINT ( 'NONE',  ( 10.92172942406178926, 54.12999999999999545, 7.935100905948387684 ) ) ;
#11821 = CARTESIAN_POINT ( 'NONE',  ( -3.239062113971910684, 71.56354731355079934, 13.10570111947281369 ) ) ;
#11822 = CARTESIAN_POINT ( 'NONE',  ( -18.62500000000064659, -2.115624999999976996, 7.714727599197333419 ) ) ;
#11823 = CARTESIAN_POINT ( 'NONE',  ( -13.49575779976988343, 67.94255581264309285, 0.3657745621878383813 ) ) ;
#11824 = CARTESIAN_POINT ( 'NONE',  ( -18.62500000000064659, -26.01562499999994671, 7.714727599197335195 ) ) ;
#11825 = CARTESIAN_POINT ( 'NONE',  ( 7.886035413494550284, 54.88256797924555030, -10.96628294449290308 ) ) ;
#11826 = VECTOR ( 'NONE', #16613, 1000.000000000000000 ) ;
#11827 = CARTESIAN_POINT ( 'NONE',  ( -9.520470885617717371, 19.22999999999999687, 6.917026985038133624 ) ) ;
#11828 = CARTESIAN_POINT ( 'NONE',  ( -13.16986379960055231, -10.40624999999997513, 13.16986379959834252 ) ) ;
#11829 = CARTESIAN_POINT ( 'NONE',  ( -11.44341903511235792, 65.19769748763089012, 7.162640882872341130 ) ) ;
#11830 = DIRECTION ( 'NONE',  ( 0.5000000000000008882, -0.000000000000000000, 0.8660254037844381525 ) ) ;
#11831 = CARTESIAN_POINT ( 'NONE',  ( -4.326545005012490286, 35.52442011644006925, 12.78817203166833316 ) ) ;
#11832 = ORIENTED_EDGE ( 'NONE', *, *, #17256, .T. ) ;
#11833 = CARTESIAN_POINT ( 'NONE',  ( -4.171729424061791036, 9.530000000000010019, 12.83926296998457239 ) ) ;
#11834 = CARTESIAN_POINT ( 'NONE',  ( -2.851258122864091415, 40.28252070923673500, -13.19546944467250960 ) ) ;
#11835 = CARTESIAN_POINT ( 'NONE',  ( -12.87226159753149268, 32.07661166022045052, 4.082475368119833803 ) ) ;
#11836 = CARTESIAN_POINT ( 'NONE',  ( 0.5300433235337840276, 73.16094159698265287, -13.48959140114411781 ) ) ;
#11837 = CARTESIAN_POINT ( 'NONE',  ( 11.64793254230706232, 60.17604334945948352, 6.824638435576549256 ) ) ;
#11838 = ADVANCED_FACE ( 'NONE', ( #17038 ), #17385, .T. ) ;
#11839 = CARTESIAN_POINT ( 'NONE',  ( -4.171729424061787483, -3.669999999999999485, -12.83926296998457417 ) ) ;
#11840 = CARTESIAN_POINT ( 'NONE',  ( -3.336379296991717869, 53.56006013931011722, 13.08240930115279710 ) ) ;
#11841 = VECTOR ( 'NONE', #13935, 1000.000000000000000 ) ;
#11842 = CARTESIAN_POINT ( 'NONE',  ( 11.76794919243112325, 61.42999999999999972, 1.441158131103945434E-15 ) ) ;
#11843 = DIRECTION ( 'NONE',  ( 0.000000000000000000, 0.000000000000000000, 1.000000000000000000 ) ) ;
#11844 = CARTESIAN_POINT ( 'NONE',  ( 13.49999999999999822, 74.28000000000000114, 4.386415899144237684 ) ) ;
#11845 = CARTESIAN_POINT ( 'NONE',  ( 13.02289043530450208, 51.30254417723856619, 3.567633519790383900 ) ) ;
#11846 = CARTESIAN_POINT ( 'NONE',  ( -11.60693306515659984, 38.18798383908444549, 6.929076632654524559 ) ) ;
#11847 = CARTESIAN_POINT ( 'NONE',  ( 12.13964550287791866, 36.64708739272366245, -5.907247546172663455 ) ) ;
#11848 = CARTESIAN_POINT ( 'NONE',  ( 8.043339635997652337, -59.28124999999987921, -8.043339635996302306 ) ) ;
#11849 = CARTESIAN_POINT ( 'NONE',  ( -5.165543354712239577, 74.49330207109468915, 12.47278248272050050 ) ) ;
#11850 = CARTESIAN_POINT ( 'NONE',  ( -12.13837278097153849, 77.14717783657690120, 5.908462373232763909 ) ) ;
#11851 = CARTESIAN_POINT ( 'NONE',  ( -6.434411898208869829, 80.44366145310867466, 11.86853559793800450 ) ) ;
#11852 = CARTESIAN_POINT ( 'NONE',  ( 7.500000000000000888, 104.9266221009244191, -8.932545650451682917 ) ) ;
#11853 = ORIENTED_EDGE ( 'NONE', *, *, #16344, .F. ) ;
#11854 = VECTOR ( 'NONE', #3909, 1000.000000000000000 ) ;
#11855 = CARTESIAN_POINT ( 'NONE',  ( 11.76794919243112325, 8.280000000000006466, 3.823638476888996163 ) ) ;
#11856 = ORIENTED_EDGE ( 'NONE', *, *, #14987, .F. ) ;
#11857 = CARTESIAN_POINT ( 'NONE',  ( 7.272992578804308828, 54.98000000000000398, 10.01041549318726886 ) ) ;
#11858 = CARTESIAN_POINT ( 'NONE',  ( 11.37499999999960565, -41.65937499999989058, 4.711679271994918317 ) ) ;
#11859 = CARTESIAN_POINT ( 'NONE',  ( 13.49999999999999822, 56.27999999999999403, 4.386415899144236796 ) ) ;
#11860 = CARTESIAN_POINT ( 'NONE',  ( -13.49999999999999822, -3.920000000000001705, 4.386415899144235908 ) ) ;
#11861 = CARTESIAN_POINT ( 'NONE',  ( 10.71234848535828199, 75.74200647849511370, -8.215984252163476498 ) ) ;
#11862 = ADVANCED_FACE ( 'NONE', ( #953 ), #2262, .T. ) ;
#11863 = CARTESIAN_POINT ( 'NONE',  ( 13.50000000000000000, 68.43000000000000682, 1.653273178848926867E-15 ) ) ;
#11864 = CARTESIAN_POINT ( 'NONE',  ( 4.171729424061791924, 70.03000000000000114, -12.83926296998457239 ) ) ;
#11865 = CARTESIAN_POINT ( 'NONE',  ( 3.636496289402157078, 38.03000000000000114, -11.19198476289190936 ) ) ;
#11866 = DIRECTION ( 'NONE',  ( 0.000000000000000000, -1.000000000000000000, 0.000000000000000000 ) ) ;
#11867 = CARTESIAN_POINT ( 'NONE',  ( -13.21369905157459890, 59.02775396092354043, 2.765669001886426059 ) ) ;
#11868 = CARTESIAN_POINT ( 'NONE',  ( 9.058805526620455240, 45.03196713883374969, 10.00967056491867524 ) ) ;
#11869 = CARTESIAN_POINT ( 'NONE',  ( 12.88435061792157832, 69.28518360341051618, 4.034773658741488411 ) ) ;
#11870 = DIRECTION ( 'NONE',  ( 0.000000000000000000, -1.000000000000000000, 0.000000000000000000 ) ) ;
#11871 = CARTESIAN_POINT ( 'NONE',  ( -4.007836095776672991, 55.32410577306614385, -12.89143502976331312 ) ) ;
#11872 = CARTESIAN_POINT ( 'NONE',  ( -8.587248194232895315, 50.35035759758954299, 10.41677944331643602 ) ) ;
#11873 = DIRECTION ( 'NONE',  ( 0.8660254037844379305, 0.000000000000000000, 0.5000000000000012212 ) ) ;
#11874 = CARTESIAN_POINT ( 'NONE',  ( 10.52133674883681813, 42.75279131939787902, -8.462481817991241329 ) ) ;
#11875 = CARTESIAN_POINT ( 'NONE',  ( 10.04801546086567399, 39.08131876964824158, 9.027590569278633126 ) ) ;
#11876 = VERTEX_POINT ( 'NONE', #4943 ) ;
#11877 = CARTESIAN_POINT ( 'NONE',  ( -6.953862414529842439, 70.43748566701286506, -11.58376311006115422 ) ) ;
#11878 = CARTESIAN_POINT ( 'NONE',  ( -9.987088467865099517, 61.57852760064511699, -9.083992418538327840 ) ) ;
#11879 = CARTESIAN_POINT ( 'NONE',  ( 11.76794919243112325, 2.430000000000015703, 1.734723475976807094E-15 ) ) ;
#11880 = VERTEX_POINT ( 'NONE', #3955 ) ;
#11881 = AXIS2_PLACEMENT_3D ( 'NONE', #8743, #14100, #1984 ) ;
#11882 = EDGE_LOOP ( 'NONE', ( #13725, #7400, #8122, #11376 ) ) ;
#11883 = CARTESIAN_POINT ( 'NONE',  ( 13.50000000000000000, 21.43000000000000327, 1.734723475976807094E-15 ) ) ;
#11884 = CARTESIAN_POINT ( 'NONE',  ( 7.714727599197338748, -46.82812499999989342, 18.62500000000063949 ) ) ;
#11885 = CARTESIAN_POINT ( 'NONE',  ( 0.6915575771887298995, 47.70484266932048456, 13.50000000000285461 ) ) ;
#11886 = ADVANCED_FACE ( 'NONE', ( #2434, #12981 ), #9284, .F. ) ;
#11887 = CARTESIAN_POINT ( 'NONE',  ( 12.45313895046523811, 57.24012120377358315, 5.212443691823386516 ) ) ;
#11888 = CARTESIAN_POINT ( 'NONE',  ( -3.636496289402153081, 71.32999999999999829, -11.19198476289190936 ) ) ;
#11889 = CARTESIAN_POINT ( 'NONE',  ( 2.272985001014427788E-15, 74.17999999999997840, -12.37355403259654985 ) ) ;
#11890 = CARTESIAN_POINT ( 'NONE',  ( -0.3885106188271407746, 47.66603124818684734, 13.49448874308720114 ) ) ;
#11891 = CARTESIAN_POINT ( 'NONE',  ( 10.92172942406179104, 41.72999999999999687, -7.935100905948385908 ) ) ;
#11892 = DIRECTION ( 'NONE',  ( -6.302562568933760152E-16, -1.000000000000000000, -0.000000000000000000 ) ) ;
#11893 = CARTESIAN_POINT ( 'NONE',  ( 4.711679271993006957, -72.87812499999979821, 11.37500000000039613 ) ) ;
#11894 = CARTESIAN_POINT ( 'NONE',  ( 2.138189944381280405, 43.75688142232026223, 13.49999999999998579 ) ) ;
#11895 = CARTESIAN_POINT ( 'NONE',  ( 7.448728434142215526, 33.90129485598647108, -11.26199948916008786 ) ) ;
#11896 = CARTESIAN_POINT ( 'NONE',  ( -2.293477329192559644, 73.26246498174589306, -13.30375830701482087 ) ) ;
#11897 = VERTEX_POINT ( 'NONE', #3606 ) ;
#11898 = VERTEX_POINT ( 'NONE', #13068 ) ;
#11899 = ORIENTED_EDGE ( 'NONE', *, *, #8576, .F. ) ;
#11900 = CARTESIAN_POINT ( 'NONE',  ( -8.343458848123582072, 17.37999999999999545, 11.48378591275254124 ) ) ;
#11901 = CARTESIAN_POINT ( 'NONE',  ( 8.043339635997652337, -59.28124999999987921, -8.043339635996302306 ) ) ;
#11902 = CARTESIAN_POINT ( 'NONE',  ( -9.960433271135549660, 44.28289197857108661, 9.113836154488136998 ) ) ;
#11903 = CARTESIAN_POINT ( 'NONE',  ( -7.499999999999995559, -27.73625732136943611, -2.063574628993723348 ) ) ;
#11904 = CARTESIAN_POINT ( 'NONE',  ( 9.771573629660572635, 66.79262956996798550, -9.315150575223826834 ) ) ;
#11905 = CARTESIAN_POINT ( 'NONE',  ( 4.171729424061791924, 40.02999999999999403, -12.83926296998457239 ) ) ;
#11906 = CARTESIAN_POINT ( 'NONE',  ( -10.23977083959674061, 71.26919422278727723, 8.841254286924575823 ) ) ;
#11907 = CARTESIAN_POINT ( 'NONE',  ( 18.62499999999934630, -98.85937499999975842, 7.714727599200467800 ) ) ;
#11908 = CARTESIAN_POINT ( 'NONE',  ( -11.89252447053387307, 68.16661037567293135, 6.393518228508523471 ) ) ;
#11909 = CARTESIAN_POINT ( 'NONE',  ( -18.62500000000064659, -18.76562499999993605, 7.714727599197333419 ) ) ;
#11910 = AXIS2_PLACEMENT_3D ( 'NONE', #10192, #2109, #7536 ) ;
#11911 = CARTESIAN_POINT ( 'NONE',  ( 5.839258915127627070, 54.96742705686380503, -12.17263519449883091 ) ) ;
#11912 = CARTESIAN_POINT ( 'NONE',  ( 18.62499999999934630, -98.85937499999975842, 7.714727599200467800 ) ) ;
#11913 = CARTESIAN_POINT ( 'NONE',  ( -12.92492960912350597, 65.06980143740064193, 3.900769340635460214 ) ) ;
#11914 = CARTESIAN_POINT ( 'NONE',  ( -1.609292034251611714, 35.62213402059252587, 13.40373931015559172 ) ) ;
#11915 = CARTESIAN_POINT ( 'NONE',  ( -4.171729424061791036, 21.52999999999999403, 12.83926296998457239 ) ) ;
#11916 = ORIENTED_EDGE ( 'NONE', *, *, #12929, .F. ) ;
#11917 = DIRECTION ( 'NONE',  ( 0.000000000000000000, 1.000000000000000000, 0.000000000000000000 ) ) ;
#11918 = CARTESIAN_POINT ( 'NONE',  ( -9.520470885617717371, 28.23000000000000398, 6.917026985038133624 ) ) ;
#11919 = CARTESIAN_POINT ( 'NONE',  ( -5.519902694494632556, 31.38019316832627581, -12.31995397698188022 ) ) ;
#11920 = DIRECTION ( 'NONE',  ( 0.000000000000000000, 0.000000000000000000, 1.000000000000000000 ) ) ;
#11921 = CARTESIAN_POINT ( 'NONE',  ( 11.63721506080949020, 60.17530159522576838, 6.842919234061048073 ) ) ;
#11922 = CARTESIAN_POINT ( 'NONE',  ( -3.892879492245595152, 53.54002628341550718, 12.92654989019562883 ) ) ;
#11923 = CARTESIAN_POINT ( 'NONE',  ( 11.76794919243112680, 58.57999999999999119, -3.823638476888993942 ) ) ;
#11924 = CARTESIAN_POINT ( 'NONE',  ( -10.92172942406179104, 73.23000000000000398, 7.935100905948387684 ) ) ;
#11925 = CARTESIAN_POINT ( 'NONE',  ( 10.68360996784106121, 51.11635650885985882, 8.252908712777312417 ) ) ;
#11926 = CARTESIAN_POINT ( 'NONE',  ( -13.10880650276811465, 37.81520070515529142, -3.229914644386858491 ) ) ;
#11927 = CARTESIAN_POINT ( 'NONE',  ( 13.04805342603775742, 36.30564934951262757, 3.492309041391611579 ) ) ;
#11928 = CARTESIAN_POINT ( 'NONE',  ( -9.552639591052204498E-13, -53.03749999999988773, 11.37499999999999645 ) ) ;
#11929 = ADVANCED_FACE ( 'NONE', ( #5124 ), #15790, .T. ) ;
#11930 = CARTESIAN_POINT ( 'NONE',  ( -6.108332572802023464, 74.45675329115508134, 12.03905252150416771 ) ) ;
#11931 = CARTESIAN_POINT ( 'NONE',  ( -2.202876632959991809, 77.60068045598771391, 13.32638450149024045 ) ) ;
#11932 = CARTESIAN_POINT ( 'NONE',  ( -12.00843261896035052, 79.70224609130038118, -6.172195262188137299 ) ) ;
#11933 = CARTESIAN_POINT ( 'NONE',  ( 3.636496289402157078, 12.03000000000001357, -11.19198476289190936 ) ) ;
#11934 = DIRECTION ( 'NONE',  ( 0.000000000000000000, -1.000000000000000000, 0.000000000000000000 ) ) ;
#11935 = EDGE_LOOP ( 'NONE', ( #7019, #9064 ) ) ;
#11936 = CARTESIAN_POINT ( 'NONE',  ( -3.636496289402156190, 7.530000000000009130, 11.19198476289190758 ) ) ;
#11937 = ORIENTED_EDGE ( 'NONE', *, *, #12229, .F. ) ;
#11938 = CARTESIAN_POINT ( 'NONE',  ( -7.272992578804310604, 57.37999999999999545, 10.01041549318726886 ) ) ;
#11939 = CARTESIAN_POINT ( 'NONE',  ( 4.711679271994911211, -45.82187499999987779, -11.37499999999960743 ) ) ;
#11940 = CARTESIAN_POINT ( 'NONE',  ( 18.62500000000000000, 0.000000000000000000, 1.560692158462880521E-12 ) ) ;
#11941 = B_SPLINE_CURVE_WITH_KNOTS ( 'NONE', 3,
 ( #8308, #6978, #2698, #12354 ),
 .UNSPECIFIED., .F., .F.,
 ( 4, 4 ),
 ( 2.376698214938428888E-07, 0.007646667280170312518 ),
 .UNSPECIFIED. ) ;
#11942 = CARTESIAN_POINT ( 'NONE',  ( -13.50000000000000000, -7.070000000000000284, -3.469446951953614189E-15 ) ) ;
#11943 = CARTESIAN_POINT ( 'NONE',  ( 6.388575815097190969, 75.94550667101978547, -11.89345360526400341 ) ) ;
#11944 = CARTESIAN_POINT ( 'NONE',  ( 13.50000000000000355, 32.57999999999999119, -4.386415899144233244 ) ) ;
#11945 = CARTESIAN_POINT ( 'NONE',  ( 10.92172942406178926, 75.12999999999999545, 7.935100905948387684 ) ) ;
#11946 = CARTESIAN_POINT ( 'NONE',  ( -7.272992578804307939, 44.47999999999999687, -10.01041549318726886 ) ) ;
#11947 = LINE ( 'NONE', #7980, #14816 ) ;
#11948 = AXIS2_PLACEMENT_3D ( 'NONE', #1234, #17406, #2721 ) ;
#11949 = CARTESIAN_POINT ( 'NONE',  ( -10.61093645061555257, 58.61191818804664422, -8.349755948771326430 ) ) ;
#11950 = DIRECTION ( 'NONE',  ( 0.000000000000000000, 0.000000000000000000, 1.000000000000000000 ) ) ;
#11951 = CARTESIAN_POINT ( 'NONE',  ( 10.80743988185431270, 69.73672264826443268, -8.091202902239265526 ) ) ;
#11952 = CARTESIAN_POINT ( 'NONE',  ( 1.732050807568877415, 7.773118517290098950, -19.00000000000000000 ) ) ;
#11953 = DIRECTION ( 'NONE',  ( 0.000000000000000000, 0.000000000000000000, 1.000000000000000000 ) ) ;
#11954 = CARTESIAN_POINT ( 'NONE',  ( -11.75435161585808785, 55.68303527114955642, -6.650987819685640901 ) ) ;
#11955 = EDGE_CURVE ( 'NONE', #1729, #12392, #5255, .T. ) ;
#11956 = CARTESIAN_POINT ( 'NONE',  ( -12.68856319678013733, 50.09667819037224490, 4.610493161354706437 ) ) ;
#11957 = CARTESIAN_POINT ( 'NONE',  ( 13.38071212497846751, 63.49259793051759004, -1.791777274255796248 ) ) ;
#11958 = CARTESIAN_POINT ( 'NONE',  ( 9.938623679662498489, 42.78404089153169565, -9.138168626435373199 ) ) ;
#11959 = CARTESIAN_POINT ( 'NONE',  ( 11.09090470402770201, 39.14001624768924614, 7.697158664951603946 ) ) ;
#11960 = EDGE_LOOP ( 'NONE', ( #14976, #12082 ) ) ;
#11961 = CARTESIAN_POINT ( 'NONE',  ( -9.884595526216783057, 70.57320152317427642, -9.194823709309879689 ) ) ;
#11962 = CARTESIAN_POINT ( 'NONE',  ( -10.06711309424234990, 61.58274721441556210, -8.994624661598212612 ) ) ;
#11963 = CARTESIAN_POINT ( 'NONE',  ( -7.272992578804310604, 1.379999999999991456, 10.01041549318726709 ) ) ;
#11964 = ORIENTED_EDGE ( 'NONE', *, *, #1587, .T. ) ;
#11965 = EDGE_LOOP ( 'NONE', ( #4828, #6429, #6247, #13151 ) ) ;
#11966 = CARTESIAN_POINT ( 'NONE',  ( 4.171729424061791924, 25.02999999999999758, -12.83926296998457239 ) ) ;
#11967 = CARTESIAN_POINT ( 'NONE',  ( 7.714727599200458030, -53.07187499999987068, -18.62499999999934985 ) ) ;
#11968 = CARTESIAN_POINT ( 'NONE',  ( 3.106396304733963554, 61.06830536267598575, -13.13775590234083879 ) ) ;
#11969 = CARTESIAN_POINT ( 'NONE',  ( 25.42428528562852819, 5.918584287042170544, 5.441113646577569796 ) ) ;
#11970 = CARTESIAN_POINT ( 'NONE',  ( 13.39815693410163000, 57.37226897754249677, 1.655122989353433605 ) ) ;
#11971 = CARTESIAN_POINT ( 'NONE',  ( -7.576616670048093940E-16, 72.68000000000000682, 12.37355403259654985 ) ) ;
#11972 = CARTESIAN_POINT ( 'NONE',  ( -9.520470885617715595, 74.62999999999999545, -6.917026985038136289 ) ) ;
#11973 = CARTESIAN_POINT ( 'NONE',  ( -11.35926100027876551, 47.20325402242907842, 7.295012114585781582 ) ) ;
#11974 = CARTESIAN_POINT ( 'NONE',  ( 4.171729424061791924, 39.03000000000000114, -12.83926296998457239 ) ) ;
#11975 = CARTESIAN_POINT ( 'NONE',  ( -2.624386480595337190, 10.00000000000000178, -12.78856375561946379 ) ) ;
#11976 = CARTESIAN_POINT ( 'NONE',  ( 9.538709233711902776E-13, -37.46249999999991331, -11.37500000000000000 ) ) ;
#11977 = ADVANCED_FACE ( 'NONE', ( #2745 ), #10731, .F. ) ;
#11978 = DIRECTION ( 'NONE',  ( -0.8660254037844418162, 0.000000000000000000, 0.4999999999999945599 ) ) ;
#11979 = CARTESIAN_POINT ( 'NONE',  ( 1.117928010715994125, 34.13984769869428249, -13.46164090031036054 ) ) ;
#11980 = CARTESIAN_POINT ( 'NONE',  ( -3.636291849404581722, 73.31075916562413397, -13.00105766639911131 ) ) ;
#11981 = ORIENTED_EDGE ( 'NONE', *, *, #8720, .T. ) ;
#11982 = EDGE_LOOP ( 'NONE', ( #16111, #7295, #15938, #38 ) ) ;
#11983 = CARTESIAN_POINT ( 'NONE',  ( -11.76794919243112325, 75.08000000000001251, 3.823638476888994830 ) ) ;
#11984 = VERTEX_POINT ( 'NONE', #11969 ) ;
#11985 = CARTESIAN_POINT ( 'NONE',  ( 11.76794919243112680, -12.42000000000000171, -3.823638476888993942 ) ) ;
#11986 = CARTESIAN_POINT ( 'NONE',  ( -8.043339635997652337, -50.95624999999989768, 8.043339635996300530 ) ) ;
#11987 = CARTESIAN_POINT ( 'NONE',  ( -4.198563671053442192, 44.52903422088949270, 12.83079698937739721 ) ) ;
#11988 = CARTESIAN_POINT ( 'NONE',  ( -7.499999999999993783, -27.68990399256867718, -2.572187159835569226 ) ) ;
#11989 = CARTESIAN_POINT ( 'NONE',  ( 13.50000000000000355, 39.57999999999998408, -4.386415899144233244 ) ) ;
#11990 = CARTESIAN_POINT ( 'NONE',  ( -3.129712353247879442, 71.56746715821304861, 13.13221255258535258 ) ) ;
#11991 = CLOSED_SHELL ( 'NONE', ( #1244, #8180, #4618, #4641, #12453, #15504, #2931, #6333, #9619, #3684, #11800, #12772, #9216, #16572, #13225, #1714, #10351, #12502, #13343, #2589, #11105, #5058, #4993, #11521, #519, #15525, #2952, #15406, #8797, #10013, #8298, #16063, #15848, #6733, #14666, #6241, #11345, #9703, #13304, #13748, #10308, #15947, #5358, #1524, #1444, #7537, #7054, #9115, #1366, #16614, #1344, #16593, #11039, #13561, #11886, #5683, #2335, #2138, #17428, #9183, #13769, #6079 ) ) ;
#11992 = CARTESIAN_POINT ( 'NONE',  ( -18.62499999999935341, -66.63437499999983515, -7.714727599200458030 ) ) ;
#11993 = CARTESIAN_POINT ( 'NONE',  ( -13.49018641668098617, 67.94809635601976083, 0.5259755334716053055 ) ) ;
#11994 = CARTESIAN_POINT ( 'NONE',  ( -7.714727599200467800, -94.69687499999979252, 18.62499999999934630 ) ) ;
#11995 = CARTESIAN_POINT ( 'NONE',  ( 0.5919370610761245377, 55.15871612706705918, -13.49999999834249387 ) ) ;
#11996 = DIRECTION ( 'NONE',  ( -0.000000000000000000, -1.000000000000000000, -0.000000000000000000 ) ) ;
#11997 = CARTESIAN_POINT ( 'NONE',  ( -13.47392021138490215, 64.90062200235198020, -0.8468760602646752123 ) ) ;
#11998 = CARTESIAN_POINT ( 'NONE',  ( -9.401475381598739745, 35.31127215530875674, 9.688255670132432940 ) ) ;
#11999 = CARTESIAN_POINT ( 'NONE',  ( -13.49999999999999822, 20.78000000000000824, -4.386415899144240349 ) ) ;
#12000 = ORIENTED_EDGE ( 'NONE', *, *, #12859, .F. ) ;
#12001 = CARTESIAN_POINT ( 'NONE',  ( 0.1739742279209033626, 1.593905776373960292E-15, -12.07604168000139033 ) ) ;
#12002 = CARTESIAN_POINT ( 'NONE',  ( -9.286222281767340547, 31.54266391133846881, -9.816746840912003336 ) ) ;
#12003 = CARTESIAN_POINT ( 'NONE',  ( 7.500000000000000888, -18.00000000000000355, 8.999999999999998224 ) ) ;
#12004 = CARTESIAN_POINT ( 'NONE',  ( -3.636496289402152637, -8.669999999999996376, -11.19198476289190936 ) ) ;
#12005 = CARTESIAN_POINT ( 'NONE',  ( 3.358410185994296082, 59.80067827238347888, 13.07579168776377010 ) ) ;
#12006 = CARTESIAN_POINT ( 'NONE',  ( 8.343458848123583849, -10.12000000000000277, -11.48378591275253768 ) ) ;
#12007 = CARTESIAN_POINT ( 'NONE',  ( -11.05360854115534863, 53.22221651762638572, 7.750340433578712052 ) ) ;
#12008 = ADVANCED_FACE ( 'NONE', ( #4925 ), #10323, .F. ) ;
#12009 = CARTESIAN_POINT ( 'NONE',  ( -11.76794919243112325, 51.07999999999999829, 3.823638476888994386 ) ) ;
#12010 = ITEM_DEFINED_TRANSFORMATION ( 'NONE', 'NONE', #16946,  #16654 ) ;
#12011 = CARTESIAN_POINT ( 'NONE',  ( -13.50000000000000000, 66.93000000000000682, -3.306546357697853733E-15 ) ) ;
#12012 = CARTESIAN_POINT ( 'NONE',  ( 3.316253209170452632, 50.79922521005602221, 13.08634827626489638 ) ) ;
#12013 = CARTESIAN_POINT ( 'NONE',  ( -10.17240047902380873, 37.58838810588826362, -8.875558754972354691 ) ) ;
#12014 = CARTESIAN_POINT ( 'NONE',  ( 9.214156735519342334, 36.03950685236531370, 9.866582668058638816 ) ) ;
#12015 = CARTESIAN_POINT ( 'NONE',  ( 7.714727599200456254, -10.37187499999999396, -18.62499999999935341 ) ) ;
#12016 = LINE ( 'NONE', #15888, #15309 ) ;
#12017 = AXIS2_PLACEMENT_3D ( 'NONE', #5239, #6218, #15009 ) ;
#12018 = CARTESIAN_POINT ( 'NONE',  ( -13.29873604195502601, 76.84834518085253308, -2.322416864990943353 ) ) ;
#12019 = CARTESIAN_POINT ( 'NONE',  ( -8.740861150229537913, 80.34329372878345055, 10.29062010435449359 ) ) ;
#12020 = CARTESIAN_POINT ( 'NONE',  ( 2.902084407815607718E-14, 5.180000000000006821, -13.50000000000000000 ) ) ;
#12021 = CYLINDRICAL_SURFACE ( 'NONE', #4401, 12.00000000000000178 ) ;
#12022 = CARTESIAN_POINT ( 'NONE',  ( -7.272992578804310604, 4.379999999999999005, 10.01041549318726709 ) ) ;
#12023 = CARTESIAN_POINT ( 'NONE',  ( -7.576616670048093940E-16, 51.68000000000000682, 12.37355403259654807 ) ) ;
#12024 = CARTESIAN_POINT ( 'NONE',  ( 9.538709233711902776E-13, -80.16249999999979536, -11.37500000000000178 ) ) ;
#12025 = CARTESIAN_POINT ( 'NONE',  ( -7.714727599197335195, -5.203124999999987566, -18.62500000000064304 ) ) ;
#12026 = CARTESIAN_POINT ( 'NONE',  ( 10.92172942406178926, -8.869999999999995666, 7.935100905948385908 ) ) ;
#12027 = CARTESIAN_POINT ( 'NONE',  ( 13.49999999999999822, 35.28000000000000114, 4.386415899144236796 ) ) ;
#12028 = CARTESIAN_POINT ( 'NONE',  ( 10.56020146213972311, 75.75055865699756907, -8.410247565123782465 ) ) ;
#12029 = CARTESIAN_POINT ( 'NONE',  ( 2.445080149700053643E-15, 33.17999999999999261, -13.50000000000000000 ) ) ;
#12030 = AXIS2_PLACEMENT_3D ( 'NONE', #16163, #1503, #5329 ) ;
#12031 = CARTESIAN_POINT ( 'NONE',  ( -11.76794919243112325, 36.08000000000000540, 3.823638476888994386 ) ) ;
#12032 = CARTESIAN_POINT ( 'NONE',  ( -4.258041676676088017, 41.52689555004522504, 12.81095024554207740 ) ) ;
#12033 = CARTESIAN_POINT ( 'NONE',  ( -8.534716217167439112, 58.50719729932798430, -10.46066808379417701 ) ) ;
#12034 = DIRECTION ( 'NONE',  ( 0.000000000000000000, 1.000000000000000000, 0.000000000000000000 ) ) ;
#12035 = CARTESIAN_POINT ( 'NONE',  ( 2.138189944381220897, 60.10311857767972299, -13.50000000000000355 ) ) ;
#12036 = CARTESIAN_POINT ( 'NONE',  ( -12.00000000000000355, 3.913974596215564539, -3.899036354794879866 ) ) ;
#12037 = CARTESIAN_POINT ( 'NONE',  ( -6.432409982582727892, 55.41626211658963541, -11.87138287464854258 ) ) ;
#12038 = CARTESIAN_POINT ( 'NONE',  ( -10.15313977396370504, 49.58728767534731219, -8.897419797724348101 ) ) ;
#12039 = CARTESIAN_POINT ( 'NONE',  ( 9.916447128233048858, 63.78514480093842565, -9.160676570550608133 ) ) ;
#12040 = CARTESIAN_POINT ( 'NONE',  ( 6.825507540484397673, 42.92779699185432918, -11.65901476425138839 ) ) ;
#12041 = CARTESIAN_POINT ( 'NONE',  ( 13.31319243190779389, 39.35139063027423845, 2.238058999171629981 ) ) ;
#12042 = PRODUCT_RELATED_PRODUCT_CATEGORY ( 'part', '', ( #4088 ) ) ;
#12043 = ORIENTED_EDGE ( 'NONE', *, *, #7024, .T. ) ;
#12044 = CARTESIAN_POINT ( 'NONE',  ( -10.95763016649321919, 70.63148440308884801, -7.897661228886724061 ) ) ;
#12045 = CARTESIAN_POINT ( 'NONE',  ( 7.999999999999904965, 0.000000000000000000, 17.32050807568881368 ) ) ;
#12046 = VECTOR ( 'NONE', #518, 1000.000000000000227 ) ;
#12047 = ORIENTED_EDGE ( 'NONE', *, *, #2287, .F. ) ;
#12048 = VERTEX_POINT ( 'NONE', #9248 ) ;
#12049 = CARTESIAN_POINT ( 'NONE',  ( 13.50000000000000355, 18.57999999999999829, -4.386415899144233244 ) ) ;
#12050 = LINE ( 'NONE', #1515, #5431 ) ;
#12051 = CARTESIAN_POINT ( 'NONE',  ( 4.764356863092740646, 61.00836482418741014, -12.63134666390240213 ) ) ;
#12052 = CARTESIAN_POINT ( 'NONE',  ( 2.621994543952811015E-15, 14.18000000000000860, -14.19474002721660355 ) ) ;
#12053 = CARTESIAN_POINT ( 'NONE',  ( 7.954458010882204277, 71.98083086217984317, 10.90864659553976956 ) ) ;
#12054 = CARTESIAN_POINT ( 'NONE',  ( 12.33862782127885716, 57.22973384493053572, 5.479451552045422780 ) ) ;
#12055 = CARTESIAN_POINT ( 'NONE',  ( 9.520470885617717371, 67.73000000000000398, -6.917026985038131848 ) ) ;
#12056 = CARTESIAN_POINT ( 'NONE',  ( -9.520470885617717371, 72.23000000000000398, 6.917026985038133624 ) ) ;
#12057 = EDGE_CURVE ( 'NONE', #4019, #16001, #15816, .T. ) ;
#12058 = CARTESIAN_POINT ( 'NONE',  ( -3.653058138417871081, 47.54865290029032110, 12.99660501964011594 ) ) ;
#12059 = CARTESIAN_POINT ( 'NONE',  ( 0.000000000000000000, 102.9300000000000068, 0.000000000000000000 ) ) ;
#12060 = CARTESIAN_POINT ( 'NONE',  ( 5.656292974072647972, -100.0000000000000000, 15.42281920893911895 ) ) ;
#12061 = CARTESIAN_POINT ( 'NONE',  ( -10.92172942406179104, 34.22999999999999687, 7.935100905948387684 ) ) ;
#12062 = CARTESIAN_POINT ( 'NONE',  ( 11.37500000000039435, -34.34062499999991047, -4.711679271993004292 ) ) ;
#12063 = LINE ( 'NONE', #5183, #17116 ) ;
#12064 = CARTESIAN_POINT ( 'NONE',  ( 12.99666601036235036, 33.56048209808822236, -3.652216699307488046 ) ) ;
#12065 = CARTESIAN_POINT ( 'NONE',  ( -1.717801689700091616, 73.24174962197940886, -13.39190774218556612 ) ) ;
#12066 = ORIENTED_EDGE ( 'NONE', *, *, #4911, .F. ) ;
#12067 = ORIENTED_EDGE ( 'NONE', *, *, #9795, .T. ) ;
#12068 = CARTESIAN_POINT ( 'NONE',  ( 9.520470885617715595, 73.12999999999999545, 6.917026985038134512 ) ) ;
#12069 = EDGE_LOOP ( 'NONE', ( #8435, #15586, #3225, #9157 ) ) ;
#12070 = CARTESIAN_POINT ( 'NONE',  ( 11.37500000000039613, -91.54062499999980673, -4.711679271993002516 ) ) ;
#12071 = LINE ( 'NONE', #12156, #13947 ) ;
#12072 = CARTESIAN_POINT ( 'NONE',  ( -7.499999999999996447, -27.80979767490545740, 0.4943161440816092322 ) ) ;
#12073 = CARTESIAN_POINT ( 'NONE',  ( -8.691771469529815392E-16, 41.67999999999998550, 14.19474002721660355 ) ) ;
#12074 = CARTESIAN_POINT ( 'NONE',  ( -13.37080425425743968, 70.99696510027449392, 1.915368337129497833 ) ) ;
#12075 = CARTESIAN_POINT ( 'NONE',  ( 7.714727599197340524, -6.278124999999967315, 18.62500000000063949 ) ) ;
#12076 = CARTESIAN_POINT ( 'NONE',  ( -12.71100910673158246, 67.76566160515973536, -4.549615297461226504 ) ) ;
#12077 = CARTESIAN_POINT ( 'NONE',  ( -18.62499999999935341, -16.68437499999993889, -7.714727599200458030 ) ) ;
#12078 = CARTESIAN_POINT ( 'NONE',  ( 11.66531418640665407, 54.17725219472052345, 6.794926229372841853 ) ) ;
#12079 = DIRECTION ( 'NONE',  ( 0.000000000000000000, 0.000000000000000000, -1.000000000000000000 ) ) ;
#12080 = CARTESIAN_POINT ( 'NONE',  ( -13.28285221338691890, 64.84474501369872712, -2.423398101427317819 ) ) ;
#12081 = CARTESIAN_POINT ( 'NONE',  ( -12.88515085615131639, 35.07508799605628980, 4.041843465557555248 ) ) ;
#12082 = ORIENTED_EDGE ( 'NONE', *, *, #15601, .F. ) ;
#12083 = DIRECTION ( 'NONE',  ( 0.000000000000000000, 0.000000000000000000, -1.000000000000000000 ) ) ;
#12084 = CARTESIAN_POINT ( 'NONE',  ( -6.905685108143932105, 31.43550380796823873, -11.61237663357330341 ) ) ;
#12085 = CARTESIAN_POINT ( 'NONE',  ( 4.867973651388805223, 73.00457954580815567, -12.59203443152197721 ) ) ;
#12086 = CARTESIAN_POINT ( 'NONE',  ( 3.636496289402154414, -10.16999999999999815, 11.19198476289190758 ) ) ;
#12087 = CARTESIAN_POINT ( 'NONE',  ( 3.238893374653856849, 59.79645227764538618, 13.10570931148826013 ) ) ;
#12088 = CARTESIAN_POINT ( 'NONE',  ( 8.343458848123578520, -5.020000000000003126, 11.48378591275254124 ) ) ;
#12089 = CARTESIAN_POINT ( 'NONE',  ( -11.95953986185622320, 53.16127550200973673, 6.262611427032776845 ) ) ;
#12090 = ADVANCED_FACE ( 'NONE', ( #10994 ), #549, .T. ) ;
#12091 = CARTESIAN_POINT ( 'NONE',  ( 3.636496289402157078, 47.02999999999999403, -11.19198476289190936 ) ) ;
#12092 = SHAPE_DEFINITION_REPRESENTATION ( #6503, #10992 ) ;
#12093 = CARTESIAN_POINT ( 'NONE',  ( 2.607531440858944223E-15, 69.18000000000000682, -14.19474002721660355 ) ) ;
#12094 = CARTESIAN_POINT ( 'NONE',  ( 11.77664224129239834, 51.18329203575517283, 6.664799459490041933 ) ) ;
#12095 = CARTESIAN_POINT ( 'NONE',  ( -6.481058573409227641, 37.41816792217149157, -11.84851559884859462 ) ) ;
#12096 = CARTESIAN_POINT ( 'NONE',  ( 8.224471913408319068, 35.99288207254014083, 10.71476016740036563 ) ) ;
#12097 = CARTESIAN_POINT ( 'NONE',  ( 18.62500000000000000, -23.89999999999996305, 1.560692158462880521E-12 ) ) ;
#12098 = CARTESIAN_POINT ( 'NONE',  ( -11.29150227822014152, 74.20758383959375237, 7.399465225293304194 ) ) ;
#12099 = CARTESIAN_POINT ( 'NONE',  ( -12.51871653938473195, 76.74630541835415443, -5.052900597489689893 ) ) ;
#12100 = CARTESIAN_POINT ( 'NONE',  ( -13.45670837459887359, 79.96812659038552340, 1.102554880423010308 ) ) ;
#12101 = CARTESIAN_POINT ( 'NONE',  ( 11.76794919243112325, 14.42999999999999794, 1.734723475976807094E-15 ) ) ;
#12102 = CARTESIAN_POINT ( 'NONE',  ( 7.500000000000000888, 107.2300670966469625, 6.927727048493004247 ) ) ;
#12103 = DIRECTION ( 'NONE',  ( 0.000000000000000000, 0.000000000000000000, -1.000000000000000000 ) ) ;
#12104 = CARTESIAN_POINT ( 'NONE',  ( 9.520470885617717371, -0.2699999999999924682, -6.917026985038131848 ) ) ;
#12105 = CARTESIAN_POINT ( 'NONE',  ( -3.636496289402155746, 48.52999999999999403, 11.19198476289190936 ) ) ;
#12106 = CARTESIAN_POINT ( 'NONE',  ( -8.043339635996302306, -22.89374999999994387, -8.043339635997654113 ) ) ;
#12107 = CARTESIAN_POINT ( 'NONE',  ( -13.16986379959834252, -22.89374999999994387, -13.16986379960055054 ) ) ;
#12108 = CARTESIAN_POINT ( 'NONE',  ( 10.92172942406179104, -5.269999999999996909, -7.935100905948385908 ) ) ;
#12109 = CARTESIAN_POINT ( 'NONE',  ( -12.01298688515180757, 40.70272110868870641, -6.163212580704716892 ) ) ;
#12110 = DIRECTION ( 'NONE',  ( -0.000000000000000000, 1.000000000000000000, -0.000000000000000000 ) ) ;
#12111 = CARTESIAN_POINT ( 'NONE',  ( 5.701800690820812534, 75.97265264077142888, -12.23843519416455550 ) ) ;
#12112 = DIRECTION ( 'NONE',  ( 0.000000000000000000, 0.000000000000000000, -1.000000000000000000 ) ) ;
#12113 =( BOUNDED_CURVE ( )  B_SPLINE_CURVE ( 2, ( #8756, #12804, #1998, #15094, #1913, #11483, #11568, #16858, #8843, #3244, #14199, #2081, #8667 ),
 .UNSPECIFIED., .F., .F. ) 
 B_SPLINE_CURVE_WITH_KNOTS ( ( 3, 2, 2, 2, 2, 2, 3 ),
 ( 0.2361111111111111049, 0.2388888888888889006, 0.2444444444444444364, 0.2500000000000000000, 0.2555555555555555358, 0.2611111111111111271, 0.2638888888888888951 ),
 .UNSPECIFIED. ) 
 CURVE ( )  GEOMETRIC_REPRESENTATION_ITEM ( )  RATIONAL_B_SPLINE_CURVE ( ( 0.9755282581475765991, 0.9755282581475765991, 1.000000000000000000, 0.9510565162951535312, 1.000000000000000000, 0.9510565162951535312, 1.000000000000000000, 0.9510565162951535312, 1.000000000000000000, 0.9510565162951535312, 1.000000000000000000, 0.9755282581475768211, 0.9755282581475768211 ) ) 
 REPRESENTATION_ITEM ( '' )  );
#12114 = CARTESIAN_POINT ( 'NONE',  ( -7.576616670048093940E-16, 39.67999999999999261, 12.37355403259654985 ) ) ;
#12115 = CARTESIAN_POINT ( 'NONE',  ( -11.18038004580210121, 41.21451517937148878, 7.566320479137822019 ) ) ;
#12116 = CARTESIAN_POINT ( 'NONE',  ( -5.755473554220444932, 58.38933414821598689, -12.21165709677288014 ) ) ;
#12117 = CARTESIAN_POINT ( 'NONE',  ( -12.00000000000000178, 9.646025403784440400, -3.899036354794879422 ) ) ;
#12118 = FACE_OUTER_BOUND ( 'NONE', #6232, .T. ) ;
#12119 = CARTESIAN_POINT ( 'NONE',  ( -7.416407864998737054, 3.613974596215562052, -10.20780970022448386 ) ) ;
#12120 = CIRCLE ( 'NONE', #14640, 1.999999999999998224 ) ;
#12121 = CARTESIAN_POINT ( 'NONE',  ( 0.000000000000000000, 0.000000000000000000, 0.000000000000000000 ) ) ;
#12122 = CARTESIAN_POINT ( 'NONE',  ( -9.962969835881040126, 49.57729431268386122, -9.110904113917294822 ) ) ;
#12123 = CARTESIAN_POINT ( 'NONE',  ( 13.40375923506036315, 63.48631738253013168, -1.615599257011282042 ) ) ;
#12124 = CARTESIAN_POINT ( 'NONE',  ( 12.20577700513132946, 42.64168893067194688, -5.771419099262523389 ) ) ;
#12125 = CARTESIAN_POINT ( 'NONE',  ( 4.286075472464928815, 38.83412300064772893, 12.80155259534364376 ) ) ;
#12126 = ORIENTED_EDGE ( 'NONE', *, *, #15163, .F. ) ;
#12127 = CARTESIAN_POINT ( 'NONE',  ( 11.00000000000001599, 7.773118517290098062, -15.58845726811988364 ) ) ;
#12128 = PLANE ( 'NONE',  #14089 ) ;
#12129 = ORIENTED_EDGE ( 'NONE', *, *, #8957, .F. ) ;
#12130 = ORIENTED_EDGE ( 'NONE', *, *, #8074, .F. ) ;
#12131 = CARTESIAN_POINT ( 'NONE',  ( 4.171729424061789260, 20.83000000000001606, 12.83926296998457239 ) ) ;
#12132 = CARTESIAN_POINT ( 'NONE',  ( 7.714727599200458030, -69.72187499999982663, -18.62499999999934985 ) ) ;
#12133 = CARTESIAN_POINT ( 'NONE',  ( 8.763194653383337140, 60.84238623439762961, -10.27162055150819064 ) ) ;
#12134 = CARTESIAN_POINT ( 'NONE',  ( -10.92172942406178926, 8.629999999999999005, -7.935100905948389460 ) ) ;
#12135 = CARTESIAN_POINT ( 'NONE',  ( 10.57835835680828929, 72.11049049234127040, 8.387854446822782251 ) ) ;
#12136 = CARTESIAN_POINT ( 'NONE',  ( 11.70212564305006353, 57.68033890375173200, -6.734146581967513256 ) ) ;
#12137 = CARTESIAN_POINT ( 'NONE',  ( 7.272992578804311492, 67.87999999999999545, -10.01041549318726709 ) ) ;
#12138 = CARTESIAN_POINT ( 'NONE',  ( -7.272992578804310604, 78.38000000000000966, 10.01041549318726709 ) ) ;
#12139 = CARTESIAN_POINT ( 'NONE',  ( -4.903230271211689306, 47.50310532243074135, 12.58596196147269808 ) ) ;
#12140 = DIRECTION ( 'NONE',  ( 0.000000000000000000, 1.000000000000000000, 0.000000000000000000 ) ) ;
#12141 = CARTESIAN_POINT ( 'NONE',  ( 10.92172942406179104, 74.73000000000000398, -7.935100905948385908 ) ) ;
#12142 = CYLINDRICAL_SURFACE ( 'NONE', #12409, 1.999999999999998224 ) ;
#12143 = CARTESIAN_POINT ( 'NONE',  ( -13.49999999999999822, 76.07999999999999829, 4.386415899144235020 ) ) ;
#12144 = CARTESIAN_POINT ( 'NONE',  ( -11.37500000000000000, -8.324999999999979750, -9.545674412382054647E-13 ) ) ;
#12145 = CARTESIAN_POINT ( 'NONE',  ( 13.50000000000000355, 6.580000000000001847, -4.386415899144233244 ) ) ;
#12146 = VECTOR ( 'NONE', #2948, 1000.000000000000000 ) ;
#12147 = CARTESIAN_POINT ( 'NONE',  ( 11.27325719286469230, 33.70873714612665140, -7.427241792320101510 ) ) ;
#12148 = CARTESIAN_POINT ( 'NONE',  ( -5.014217190436002447, 73.36095352106737266, -12.53426255818751933 ) ) ;
#12149 = ORIENTED_EDGE ( 'NONE', *, *, #6438, .F. ) ;
#12150 = EDGE_CURVE ( 'NONE', #14160, #14568, #8352, .T. ) ;
#12151 = ORIENTED_EDGE ( 'NONE', *, *, #15881, .T. ) ;
#12152 = CARTESIAN_POINT ( 'NONE',  ( -3.636496289402152637, 18.33000000000001251, -11.19198476289190936 ) ) ;
#12153 = DIRECTION ( 'NONE',  ( -9.637352644315595243E-17, 1.000000000000000000, 0.000000000000000000 ) ) ;
#12154 = ORIENTED_EDGE ( 'NONE', *, *, #4516, .F. ) ;
#12155 = CARTESIAN_POINT ( 'NONE',  ( 4.711679271993006957, -87.37812499999982663, 11.37500000000039257 ) ) ;
#12156 = CARTESIAN_POINT ( 'NONE',  ( 7.500000000000000000, -28.00000000000000000, 9.367496997597600128 ) ) ;
#12157 = CARTESIAN_POINT ( 'NONE',  ( 9.658320279281740639, 8.027799056124987231, 15.34211313687883660 ) ) ;
#12158 = CARTESIAN_POINT ( 'NONE',  ( -8.691771469529815392E-16, 47.67999999999999972, 14.19474002721660355 ) ) ;
#12159 = CARTESIAN_POINT ( 'NONE',  ( -13.49999999999999822, 49.07999999999999829, 4.386415899144235908 ) ) ;
#12160 = CARTESIAN_POINT ( 'NONE',  ( -13.39839221111840750, 70.87233709335372112, -1.653208847849865215 ) ) ;
#12161 = CARTESIAN_POINT ( 'NONE',  ( -18.62500000000064659, -18.76562499999993605, 7.714727599197333419 ) ) ;
#12162 = B_SPLINE_CURVE_WITH_KNOTS ( 'NONE', 3,
 ( #13676, #9647, #3071, #14028, #261, #11224, #16329, #8497, #7076, #15080 ),
 .UNSPECIFIED., .F., .F.,
 ( 4, 2, 2, 2, 4 ),
 ( 2.344023999695694731E-07, 0.0005276420589627702547, 0.001055049715525570829, 0.001582457372088371620, 0.002109865028651171977 ),
 .UNSPECIFIED. ) ;
#12163 = CARTESIAN_POINT ( 'NONE',  ( -12.07707027602519112, 68.15293157428645543, 6.055626961436693101 ) ) ;
#12164 = CARTESIAN_POINT ( 'NONE',  ( 18.62500000000000000, -99.89999999999976410, 1.560692158462880521E-12 ) ) ;
#12165 = CARTESIAN_POINT ( 'NONE',  ( 12.98848230150326621, 54.56155940439027319, -3.680959392705737798 ) ) ;
#12166 = CARTESIAN_POINT ( 'NONE',  ( -11.76794919243112325, 16.08000000000000895, 3.823638476888994386 ) ) ;
#12167 = CYLINDRICAL_SURFACE ( 'NONE', #255, 4.000000000000000000 ) ;
#12168 = CARTESIAN_POINT ( 'NONE',  ( -13.46209291828269983, 64.89500517973988281, -1.010990238245216943 ) ) ;
#12169 = EDGE_CURVE ( 'NONE', #2917, #5695, #16362, .T. ) ;
#12170 = CARTESIAN_POINT ( 'NONE',  ( -12.47073097209211667, 35.11824904818834625, 5.170595160201629348 ) ) ;
#12171 = CARTESIAN_POINT ( 'NONE',  ( -4.171729424061787483, 20.33000000000001606, -12.83926296998457417 ) ) ;
#12172 = EDGE_LOOP ( 'NONE', ( #14699, #8192 ) ) ;
#12173 = CARTESIAN_POINT ( 'NONE',  ( -11.58348967342891633, 9.630592963500571476E-15, -5.893907634779756322 ) ) ;
#12174 = CARTESIAN_POINT ( 'NONE',  ( -10.97962057844975270, 31.63274308883676156, -7.866999682609990607 ) ) ;
#12175 = CARTESIAN_POINT ( 'NONE',  ( 5.975404689433335470, 72.96202560524248781, -12.10557300981717610 ) ) ;
#12176 = CARTESIAN_POINT ( 'NONE',  ( 9.520470885617715595, -12.86999999999999922, 6.917026985038135400 ) ) ;
#12177 = DIRECTION ( 'NONE',  ( -1.000000000000000000, -0.000000000000000000, -0.000000000000000000 ) ) ;
#12178 = CARTESIAN_POINT ( 'NONE',  ( 13.50000000000000000, -16.57000000000000028, 1.734723475976807094E-15 ) ) ;
#12179 = CARTESIAN_POINT ( 'NONE',  ( -12.78222371368175914, 52.77349219538730551, -4.343505285234531499 ) ) ;
#12180 = CARTESIAN_POINT ( 'NONE',  ( 7.272992578804311492, 46.87999999999998835, -10.01041549318726709 ) ) ;
#12181 = CARTESIAN_POINT ( 'NONE',  ( -13.49999999999999822, 66.78000000000001535, -4.386415899144240349 ) ) ;
#12182 = CARTESIAN_POINT ( 'NONE',  ( 3.303023401292605854, 50.79875792230046017, 13.08969376897518266 ) ) ;
#12183 = CARTESIAN_POINT ( 'NONE',  ( -11.52100015834348490, 37.66715461419663313, -7.042761957645991444 ) ) ;
#12184 = CARTESIAN_POINT ( 'NONE',  ( 4.071488193451239468, 35.82639234911870574, 12.87155199998092314 ) ) ;
#12185 = CARTESIAN_POINT ( 'NONE',  ( -9.552639591052204498E-13, -86.33749999999982094, 11.37499999999999645 ) ) ;
#12186 = CARTESIAN_POINT ( 'NONE',  ( -11.27694939588988099, 74.20849020820207897, 7.421620996757082978 ) ) ;
#12187 = CARTESIAN_POINT ( 'NONE',  ( -9.953402372925438613, 76.57636814536873260, -9.131542486324162766 ) ) ;
#12188 = EDGE_CURVE ( 'NONE', #13982, #13489, #3149, .T. ) ;
#12189 = CARTESIAN_POINT ( 'NONE',  ( -6.552499304188867058, 79.42106022813749178, -11.80367691769144578 ) ) ;
#12190 = CARTESIAN_POINT ( 'NONE',  ( -10.16154112308408664, 80.92999999999997840, 6.935345943047934725 ) ) ;
#12191 = CARTESIAN_POINT ( 'NONE',  ( -8.291044507619272909E-14, 7.180000000000005045, -13.50000000000000000 ) ) ;
#12192 = CARTESIAN_POINT ( 'NONE',  ( -9.520470885617717371, 4.230000000000011084, 6.917026985038133624 ) ) ;
#12193 = CARTESIAN_POINT ( 'NONE',  ( -7.576616670048093940E-16, 45.67999999999999261, 12.37355403259654807 ) ) ;
#12194 = CARTESIAN_POINT ( 'NONE',  ( -8.043339635997654113, -43.70624999999989768, 8.043339635996302306 ) ) ;
#12195 = CARTESIAN_POINT ( 'NONE',  ( -7.714727599197335195, -38.50312499999991189, -18.62500000000064304 ) ) ;
#12196 = CARTESIAN_POINT ( 'NONE',  ( -8.343458848123582072, -12.62000000000000277, 11.48378591275254124 ) ) ;
#12197 = CARTESIAN_POINT ( 'NONE',  ( -11.90770218001530978, 40.69479922003479544, -6.360556165360144121 ) ) ;
#12198 = AXIS2_PLACEMENT_3D ( 'NONE', #3586, #9506, #17021 ) ;
#12199 = CARTESIAN_POINT ( 'NONE',  ( 10.99999999999990941, 0.000000000000000000, 15.58845726811995824 ) ) ;
#12200 = CARTESIAN_POINT ( 'NONE',  ( 10.23922769745222006, 75.09193609827978833, 8.798267285036342145 ) ) ;
#12201 = CARTESIAN_POINT ( 'NONE',  ( 16.98133590665164760, 1.089405092048506085E-13, -7.261809523205409178 ) ) ;
#12202 = CARTESIAN_POINT ( 'NONE',  ( -2.104796621658385103, 41.60471069576241376, 13.35964989392017266 ) ) ;
#12203 = CARTESIAN_POINT ( 'NONE',  ( -4.329453876402491019, 58.33570365221549281, -12.78742087842741881 ) ) ;
#12204 = CARTESIAN_POINT ( 'NONE',  ( 3.025992313210662754, 44.78877108066809853, 13.15667717828717365 ) ) ;
#12205 = CARTESIAN_POINT ( 'NONE',  ( 0.000000000000000000, 80.93000000000000682, 0.000000000000000000 ) ) ;
#12206 = DIRECTION ( 'NONE',  ( 0.000000000000000000, -0.000000000000000000, -1.000000000000000000 ) ) ;
#12207 = DIRECTION ( 'NONE',  ( 0.000000000000000000, 0.000000000000000000, -1.000000000000000000 ) ) ;
#12208 = CARTESIAN_POINT ( 'NONE',  ( -11.75516853449998855, 49.68309035655853734, -6.649812433528813571 ) ) ;
#12209 = CARTESIAN_POINT ( 'NONE',  ( 13.47201310395382201, 63.39998930646792275, 0.8689103304181599041 ) ) ;
#12210 = CARTESIAN_POINT ( 'NONE',  ( 12.21953790584814570, 42.21938887054512435, 5.740768505231178764 ) ) ;
#12211 = CARTESIAN_POINT ( 'NONE',  ( -18.71141623506676410, 7.854708462831349713, -1.539237008743911339 ) ) ;
#12212 = VERTEX_POINT ( 'NONE', #12403 ) ;
#12213 = CARTESIAN_POINT ( 'NONE',  ( 0.000000000000000000, -22.00000000000000000, 0.000000000000000000 ) ) ;
#12214 = CARTESIAN_POINT ( 'NONE',  ( 9.538709233711902776E-13, -4.162499999999988987, -11.37500000000000000 ) ) ;
#12215 = CARTESIAN_POINT ( 'NONE',  ( 8.343458848123578520, 14.98000000000000043, 11.48378591275254124 ) ) ;
#12216 = ORIENTED_EDGE ( 'NONE', *, *, #13084, .T. ) ;
#12217 = CARTESIAN_POINT ( 'NONE',  ( -7.856066726180596760, 43.47605057973713372, -11.00250018620803161 ) ) ;
#12218 = CARTESIAN_POINT ( 'NONE',  ( -7.499999999999999112, 107.2300670966469340, -6.927727048493005135 ) ) ;
#12219 = CARTESIAN_POINT ( 'NONE',  ( 9.199277144405600737, 60.82129824580783861, -9.880725865329580415 ) ) ;
#12220 =( BOUNDED_CURVE ( )  B_SPLINE_CURVE ( 2, ( #13840, #7154, #12539, #12884, #8751, #3423, #16938, #937, #3505, #14277, #1993, #772, #3590 ),
 .UNSPECIFIED., .F., .F. ) 
 B_SPLINE_CURVE_WITH_KNOTS ( ( 3, 2, 2, 2, 2, 2, 3 ),
 ( 0.1249999999999999861, 0.1277777777777777679, 0.1333333333333333315, 0.1388888888888888951, 0.1444444444444444309, 0.1499999999999999944, 0.1527777777777777624 ),
 .UNSPECIFIED. ) 
 CURVE ( )  GEOMETRIC_REPRESENTATION_ITEM ( )  RATIONAL_B_SPLINE_CURVE ( ( 0.9755282581475768211, 0.9755282581475768211, 1.000000000000000000, 0.9510565162951535312, 1.000000000000000000, 0.9510565162951535312, 1.000000000000000000, 0.9510565162951535312, 1.000000000000000000, 0.9510565162951535312, 1.000000000000000000, 0.9755282581475768211, 0.9755282581475765991 ) ) 
 REPRESENTATION_ITEM ( '' )  );
#12221 = CARTESIAN_POINT ( 'NONE',  ( 4.171729424061791924, 8.030000000000010019, -12.83926296998457239 ) ) ;
#12222 = CIRCLE ( 'NONE', #4883, 8.999999999999998224 ) ;
#12223 = CARTESIAN_POINT ( 'NONE',  ( 7.614339970345533892, 71.96589283257024761, 11.14773206480789902 ) ) ;
#12224 = CARTESIAN_POINT ( 'NONE',  ( 11.63364995522154111, 66.68500620773784249, -6.849007341775995350 ) ) ;
#12225 = CARTESIAN_POINT ( 'NONE',  ( 5.049197031033813232, 56.86226893306975683, 12.52026344672814773 ) ) ;
#12226 = CARTESIAN_POINT ( 'NONE',  ( 11.76794919243112325, 70.28000000000000114, 3.823638476888996607 ) ) ;
#12227 = CARTESIAN_POINT ( 'NONE',  ( 11.76794919243112325, 64.43000000000000682, 1.441158131103945434E-15 ) ) ;
#12228 = CARTESIAN_POINT ( 'NONE',  ( -11.35148106077255292, 47.20374464058922825, 7.307114632781469332 ) ) ;
#12229 = EDGE_CURVE ( 'NONE', #16027, #15567, #894, .T. ) ;
#12230 = CARTESIAN_POINT ( 'NONE',  ( 0.000000000000000000, 0.000000000000000000, 0.000000000000000000 ) ) ;
#12231 = CARTESIAN_POINT ( 'NONE',  ( 1.156690518843624726, 7.956351059191330677, -18.35912573876699838 ) ) ;
#12232 = CARTESIAN_POINT ( 'NONE',  ( 13.22006015585995797, -99.99999999999995737, 12.20452656438226846 ) ) ;
#12233 = CARTESIAN_POINT ( 'NONE',  ( -3.432968479904499937, 56.55653457480887170, 13.05682199246169439 ) ) ;
#12234 = CARTESIAN_POINT ( 'NONE',  ( 9.538709233711902776E-13, -54.11249999999986926, -11.37500000000000000 ) ) ;
#12235 = CARTESIAN_POINT ( 'NONE',  ( -10.92172942406178926, 39.62999999999999545, -7.935100905948389460 ) ) ;
#12236 = CARTESIAN_POINT ( 'NONE',  ( 13.05193165377879971, 33.55293093225556333, -3.449255337325025650 ) ) ;
#12237 = CARTESIAN_POINT ( 'NONE',  ( 6.714875219186475341, 9.999999999999998224, 11.61066632034327029 ) ) ;
#12238 = CARTESIAN_POINT ( 'NONE',  ( -1.245860404445607248E-06, 40.18000018109674443, -13.49999999999994316 ) ) ;
#12239 = VERTEX_POINT ( 'NONE', #8440 ) ;
#12240 = CARTESIAN_POINT ( 'NONE',  ( -2.502312991112111806, 62.59002693677476259, 13.26656818365915846 ) ) ;
#12241 = ORIENTED_EDGE ( 'NONE', *, *, #7816, .F. ) ;
#12242 = CARTESIAN_POINT ( 'NONE',  ( -13.47712500954352421, 40.90289342314857635, -0.7855927258160574356 ) ) ;
#12243 = CARTESIAN_POINT ( 'NONE',  ( -4.711679271994915652, -68.64687499999988063, 11.37499999999960210 ) ) ;
#12244 = CARTESIAN_POINT ( 'NONE',  ( -11.97926611549661935, 44.15976937875102948, 6.224998469355170094 ) ) ;
#12245 = CARTESIAN_POINT ( 'NONE',  ( 10.35822530491745219, 7.924527530346062498, 15.34527529650336142 ) ) ;
#12246 = CARTESIAN_POINT ( 'NONE',  ( -10.92172942406178926, 43.62999999999999545, -7.935100905948389460 ) ) ;
#12247 = CARTESIAN_POINT ( 'NONE',  ( 10.92172942406178926, 47.12999999999999545, 7.935100905948387684 ) ) ;
#12248 = CARTESIAN_POINT ( 'NONE',  ( -12.90636597786267004, 71.07200195134710441, 3.959650672786486414 ) ) ;
#12249 = CARTESIAN_POINT ( 'NONE',  ( 1.561832610794586740E-12, -63.51249999999981810, -18.62500000000000000 ) ) ;
#12250 = CARTESIAN_POINT ( 'NONE',  ( -8.282215288612736259, 67.49552574882251577, -10.66482282856927988 ) ) ;
#12251 = CARTESIAN_POINT ( 'NONE',  ( -7.714727599197334307, -81.20312499999978684, -18.62500000000064659 ) ) ;
#12252 = CARTESIAN_POINT ( 'NONE',  ( 12.61908122025767831, 54.25491345416680389, 4.836902432757269388 ) ) ;
#12253 = CARTESIAN_POINT ( 'NONE',  ( -12.93929638727112774, 64.79209698274094364, -3.850488161051479175 ) ) ;
#12254 = ORIENTED_EDGE ( 'NONE', *, *, #696, .T. ) ;
#12255 = CARTESIAN_POINT ( 'NONE',  ( 5.441113646577481866, 0.000000000000000000, -25.42428528562854595 ) ) ;
#12256 = CARTESIAN_POINT ( 'NONE',  ( -12.15349527366901583, 34.71354853195965262, -5.893693796836648957 ) ) ;
#12257 = EDGE_LOOP ( 'NONE', ( #5630, #4725, #17076, #12066 ) ) ;
#12258 = CARTESIAN_POINT ( 'NONE',  ( 12.77063822339987986, 78.27209968102339133, 4.380528554209194958 ) ) ;
#12259 = CARTESIAN_POINT ( 'NONE',  ( -13.41004031202893465, -1.988777493506883524E-15, 1.025385998934613463 ) ) ;
#12260 = CARTESIAN_POINT ( 'NONE',  ( -10.19389412933198891, 31.58943635166178865, -8.850721524905974746 ) ) ;
#12261 = CARTESIAN_POINT ( 'NONE',  ( 10.30697988259215059, 72.76444513209375486, -8.718751012341657614 ) ) ;
#12262 = CARTESIAN_POINT ( 'NONE',  ( -7.272992578804310604, -7.620000000000000995, 10.01041549318726709 ) ) ;
#12263 = CARTESIAN_POINT ( 'NONE',  ( 5.014896044935506225, 59.86097445767614289, 12.53416570668548147 ) ) ;
#12264 = CARTESIAN_POINT ( 'NONE',  ( 4.171729424061789260, -14.17000000000000171, 12.83926296998457239 ) ) ;
#12265 = CARTESIAN_POINT ( 'NONE',  ( -8.691771469529815392E-16, 71.68000000000000682, 14.19474002721660355 ) ) ;
#12266 = CARTESIAN_POINT ( 'NONE',  ( -11.37807240653128105, 52.65795867555990384, -7.266101496908787816 ) ) ;
#12267 = CARTESIAN_POINT ( 'NONE',  ( -9.520470885617717371, 45.22999999999999687, 6.917026985038133624 ) ) ;
#12268 = CARTESIAN_POINT ( 'NONE',  ( -10.92172942406179104, 70.23000000000000398, 7.935100905948387684 ) ) ;
#12269 = EDGE_CURVE ( 'NONE', #7861, #5802, #1693, .T. ) ;
#12270 = CARTESIAN_POINT ( 'NONE',  ( -16.47957145870423901, 7.956016782093530360, -8.177092975169026445 ) ) ;
#12271 = CARTESIAN_POINT ( 'NONE',  ( 10.89610398280023595, 69.73159480780164188, -7.971896094627922480 ) ) ;
#12272 = CARTESIAN_POINT ( 'NONE',  ( -5.373303095793861672, 37.37454771265330322, -12.38528482517545015 ) ) ;
#12273 = CARTESIAN_POINT ( 'NONE',  ( 4.326442524531895373, 35.83557250899896474, 12.78850620315103015 ) ) ;
#12274 = CARTESIAN_POINT ( 'NONE',  ( 13.16986379960055409, -42.63124999999990905, -13.16986379959834430 ) ) ;
#12275 = CARTESIAN_POINT ( 'NONE',  ( -6.199815743880803254, 74.45309725584640148, 11.99228407210806147 ) ) ;
#12276 = PRODUCT ( 'Nut', 'Nut', '', ( #6630 ) ) ;
#12277 = CARTESIAN_POINT ( 'NONE',  ( -12.53661919023033811, 76.74802840221525457, -5.008329300253832272 ) ) ;
#12278 = CARTESIAN_POINT ( 'NONE',  ( -12.79019475395541505, 80.08649566584584534, 4.342692408574423624 ) ) ;
#12279 = CARTESIAN_POINT ( 'NONE',  ( 9.520470885617717371, 11.73000000000000398, -6.917026985038131848 ) ) ;
#12280 = DIRECTION ( 'NONE',  ( 0.000000000000000000, -1.000000000000000000, 0.000000000000000000 ) ) ;
#12281 = CARTESIAN_POINT ( 'NONE',  ( -7.686450350235888962, 80.93000000000003524, 9.894994522812504911 ) ) ;
#12282 = CARTESIAN_POINT ( 'NONE',  ( 13.50000000000000000, 28.43000000000001037, 1.734723475976807094E-15 ) ) ;
#12283 = CARTESIAN_POINT ( 'NONE',  ( -11.76794919243112325, -1.920000000000006590, 3.823638476888994386 ) ) ;
#12284 = CARTESIAN_POINT ( 'NONE',  ( 11.76794919243112325, 43.28000000000000114, 3.823638476888997051 ) ) ;
#12285 = CARTESIAN_POINT ( 'NONE',  ( -13.50000000000000000, -16.06999999999999318, -3.469446951953614189E-15 ) ) ;
#12286 = CARTESIAN_POINT ( 'NONE',  ( -5.574510941783231033, 40.38230122635308561, -12.29535200136428053 ) ) ;
#12287 = CARTESIAN_POINT ( 'NONE',  ( -2.720355926141545755, 34.27781377822991971, -13.22308644890100027 ) ) ;
#12288 = CARTESIAN_POINT ( 'NONE',  ( 13.48856620667041817, 75.44918483557830768, -0.5573347285596893519 ) ) ;
#12289 = CARTESIAN_POINT ( 'NONE',  ( 3.816460439845750230, 8.305967389184013400E-17, -15.37564352525922473 ) ) ;
#12290 =( NAMED_UNIT ( * ) PLANE_ANGLE_UNIT ( ) SI_UNIT ( $, .RADIAN. ) );
#12291 = CARTESIAN_POINT ( 'NONE',  ( -10.79260502828427448, 41.23832797851595444, 8.135719096258426930 ) ) ;
#12292 = EDGE_CURVE ( 'NONE', #14612, #11330, #9392, .T. ) ;
#12293 = CARTESIAN_POINT ( 'NONE',  ( -8.793690106930448280, 58.51931832914060294, -10.24309792423728638 ) ) ;
#12294 = CARTESIAN_POINT ( 'NONE',  ( 5.517797477233192360, 44.87981964034685234, 12.33095150429005571 ) ) ;
#12295 =( REPRESENTATION_RELATIONSHIP ('NONE','NONE', #7275, #4322 ) REPRESENTATION_RELATIONSHIP_WITH_TRANSFORMATION ( #7957 )SHAPE_REPRESENTATION_RELATIONSHIP( ) );
#12296 = DIRECTION ( 'NONE',  ( 0.000000000000000000, -1.000000000000000000, 0.000000000000000000 ) ) ;
#12297 = CYLINDRICAL_SURFACE ( 'NONE', #6775, 4.000000000000000000 ) ;
#12298 = CARTESIAN_POINT ( 'NONE',  ( -13.49999999999999822, 58.07999999999999119, 4.386415899144235020 ) ) ;
#12299 = CARTESIAN_POINT ( 'NONE',  ( -13.46636358844568804, 49.89703890068803105, -0.9552207532122933831 ) ) ;
#12300 = CARTESIAN_POINT ( 'NONE',  ( 12.71497711639302430, 63.59386036163260059, -4.536661660007360375 ) ) ;
#12301 = CARTESIAN_POINT ( 'NONE',  ( 13.27852674175506387, 42.34417970882014970, 2.437829359112944960 ) ) ;
#12302 = CARTESIAN_POINT ( 'NONE',  ( 1.360536668025988272, 38.72891990362956705, 13.43129604877473326 ) ) ;
#12303 = ORIENTED_EDGE ( 'NONE', *, *, #14837, .F. ) ;
#12304 = CARTESIAN_POINT ( 'NONE',  ( -1.900613283894433181, 3.122906826104708600, -12.00000000000000000 ) ) ;
#12305 = CARTESIAN_POINT ( 'NONE',  ( 11.37499999999960210, -15.60937499999996270, 4.711679271994917428 ) ) ;
#12306 = CARTESIAN_POINT ( 'NONE',  ( -8.549982208541774191E-16, 14.68000000000000682, 14.19474002721660355 ) ) ;
#12307 = ORIENTED_EDGE ( 'NONE', *, *, #9500, .F. ) ;
#12308 = CARTESIAN_POINT ( 'NONE',  ( -5.664360417381419488, 43.38578491710213569, -12.25418510808193240 ) ) ;
#12309 = CARTESIAN_POINT ( 'NONE',  ( -7.500000000000000000, 108.7397976749054891, -0.4943161440816168373 ) ) ;
#12310 = CARTESIAN_POINT ( 'NONE',  ( 13.19392137637406925, 60.53158643750810342, -2.870547323392556915 ) ) ;
#12311 = MECHANICAL_DESIGN_GEOMETRIC_PRESENTATION_REPRESENTATION (  '', ( #8657 ), #3265 ) ;
#12312 = CARTESIAN_POINT ( 'NONE',  ( 10.92172942406179104, 7.730000000000014637, -7.935100905948385908 ) ) ;
#12313 = CARTESIAN_POINT ( 'NONE',  ( -12.00000000000000178, 6.946025403784437557, 3.899036354794875869 ) ) ;
#12314 = CARTESIAN_POINT ( 'NONE',  ( 13.38999116389189936, 66.49008748670826208, -1.721341902523813472 ) ) ;
#12315 = CARTESIAN_POINT ( 'NONE',  ( 2.437340764247437175, 56.76768723153878682, 13.28085166176790288 ) ) ;
#12316 = CARTESIAN_POINT ( 'NONE',  ( 11.76794919243112325, 58.42999999999999261, 1.441158131103945434E-15 ) ) ;
#12317 = CARTESIAN_POINT ( 'NONE',  ( -4.171729424061787483, 36.32999999999999829, -12.83926296998457417 ) ) ;
#12318 = CARTESIAN_POINT ( 'NONE',  ( 3.636496289402157078, 65.03000000000000114, -11.19198476289190936 ) ) ;
#12319 = CARTESIAN_POINT ( 'NONE',  ( -7.060864377102370248, 47.41778540159006639, 11.50630388396855075 ) ) ;
#12320 = CARTESIAN_POINT ( 'NONE',  ( 2.785878927130813844E-06, 56.68007738487546732, 13.49999999999942979 ) ) ;
#12321 = CARTESIAN_POINT ( 'NONE',  ( 12.00000000000006395, 8.713974596215594559, -3.899036354794894521 ) ) ;
#12322 = CARTESIAN_POINT ( 'NONE',  ( 18.62362042714189059, -100.0000000000000000, 0.000000000000000000 ) ) ;
#12323 = CARTESIAN_POINT ( 'NONE',  ( -8.656036233252274670, 56.34715074576422467, 10.35972221486941791 ) ) ;
#12324 = CARTESIAN_POINT ( 'NONE',  ( -8.043339635997654113, -43.70624999999989768, 8.043339635996302306 ) ) ;
#12325 = CARTESIAN_POINT ( 'NONE',  ( -10.92172942406179104, 40.23000000000000398, 7.935100905948387684 ) ) ;
#12326 = CARTESIAN_POINT ( 'NONE',  ( 11.60125947145433045, 33.68733103568060017, -6.906614582173877359 ) ) ;
#12327 = CARTESIAN_POINT ( 'NONE',  ( -4.928896808027950271, 9.999999999999994671, 11.62321627039424321 ) ) ;
#12328 = DIRECTION ( 'NONE',  ( 0.000000000000000000, 0.000000000000000000, 1.000000000000000000 ) ) ;
#12329 = CARTESIAN_POINT ( 'NONE',  ( -5.609107424940139808, 62.47635901954124904, 12.27957684733320320 ) ) ;
#12330 =( BOUNDED_CURVE ( )  B_SPLINE_CURVE ( 2, ( #12437, #8386, #240, #323, #16214, #5646, #1375, #14885, #2780, #8210, #13572, #1464, #9626 ),
 .UNSPECIFIED., .F., .F. ) 
 B_SPLINE_CURVE_WITH_KNOTS ( ( 3, 2, 2, 2, 2, 2, 3 ),
 ( 0.3750000000000000000, 0.3777777777777777679, 0.3833333333333333592, 0.3888888888888888951, 0.3944444444444444309, 0.4000000000000000222, 0.4027777777777777901 ),
 .UNSPECIFIED. ) 
 CURVE ( )  GEOMETRIC_REPRESENTATION_ITEM ( )  RATIONAL_B_SPLINE_CURVE ( ( 0.9755282581475768211, 0.9755282581475768211, 1.000000000000000000, 0.9510565162951535312, 1.000000000000000000, 0.9510565162951535312, 1.000000000000000000, 0.9510565162951535312, 1.000000000000000000, 0.9510565162951535312, 1.000000000000000000, 0.9755282581475768211, 0.9755282581475768211 ) ) 
 REPRESENTATION_ITEM ( '' )  );
#12331 = ORIENTED_EDGE ( 'NONE', *, *, #16246, .F. ) ;
#12332 = CARTESIAN_POINT ( 'NONE',  ( 3.636496289402154414, -13.17000000000000171, 11.19198476289190758 ) ) ;
#12333 = CARTESIAN_POINT ( 'NONE',  ( 13.16986379960055409, -59.28124999999987921, -13.16986379959834430 ) ) ;
#12334 = EDGE_CURVE ( 'NONE', #10449, #8975, #1608, .T. ) ;
#12335 = CARTESIAN_POINT ( 'NONE',  ( -13.46460360472914886, 43.89619422539368543, -0.9770138388471342195 ) ) ;
#12336 = CARTESIAN_POINT ( 'NONE',  ( 4.171729424061791924, 1.030000000000003135, -12.83926296998457239 ) ) ;
#12337 = CIRCLE ( 'NONE', #7835, 8.999999999999998224 ) ;
#12338 = CARTESIAN_POINT ( 'NONE',  ( -4.171729424061791036, 38.52999999999999403, 12.83926296998457239 ) ) ;
#12339 = CARTESIAN_POINT ( 'NONE',  ( 10.92172942406179104, 44.72999999999999687, -7.935100905948385908 ) ) ;
#12340 = CARTESIAN_POINT ( 'NONE',  ( -13.47028805993524259, 70.89819967500132236, -0.9202425323688597780 ) ) ;
#12341 = CARTESIAN_POINT ( 'NONE',  ( -7.714727599200466912, -70.79687499999981526, 18.62499999999935341 ) ) ;
#12342 = CARTESIAN_POINT ( 'NONE',  ( -10.97285289887956417, 67.63299039756994091, -7.864268408584646153 ) ) ;
#12343 = CARTESIAN_POINT ( 'NONE',  ( 13.16986379960055409, -61.43124999999983515, -13.16986379959834430 ) ) ;
#12344 = B_SPLINE_CURVE_WITH_KNOTS ( 'NONE', 3,
 ( #10853, #16221, #11035, #4133, #14894, #1647, #6237, #3567, #7063, #13747, #12445, #4818, #15657, #330, #8483, #5739, #11120, #14169, #15572, #8982, #16494, #15156, #14337, #12861, #4399, #15488, #9810, #3054, #7147, #11452, #750, #16999, #825, #12771, #2226, #7655, #3483, #13031, #3398, #13834, #915, #8897, #1734, #2056, #660, #8811, #14252, #10394, #6069, #6324, #16826, #4733, #10134, #11624, #11710, #7480, #6158, #11535, #10219, #17087, #16913, #2140, #7565, #12942, #4905, #10304, #4992, #2964, #8394, #11799, #7741, #3659, #2313, #9071, #15749, #13116, #1004, #6415, #17176, #14424, #5087, #16488, #14889, #14979, #15062, #16666, #9629, #4395, #3140, #4573, #153, #8479, #13918, #12350, #4485, #413, #16309, #12440, #13659, #5559, #6972, #244, #11288, #5649, #11205, #8213, #11030, #1553, #16402, #2783, #4304, #9716, #13575, #15152, #10943, #1730, #2960, #9805, #13743, #326, #4216, #5821, #1467, #16580, #6886, #12258, #8565, #2871, #8303, #3050, #8390, #7143, #1643, #7059, #9894, #5910, #5735, #11116, #15242, #13830, #503, #12529, #1812, #7226, #12612, #1982, #8912, #14005, #1898, #11380, #17017, #2241, #8739, #16752, #8651, #4746, #15590, #17102, #7316, #10319, #12700, #15417, #4660, #7407, #8995, #12789, #14097, #7669, #10152, #675, #6252, #3324, #3231, #587, #11638, #6087, #10067, #11467, #16843, #4921, #2069, #15674, #13048, #3582, #8826 ),
 .UNSPECIFIED., .F., .F.,
 ( 4, 2, 1, 1, 1, 2, 2, 2, 2, 1, 2, 2, 1, 2, 1, 1, 1, 2, 2, 1, 2, 2, 2, 1, 1, 1, 2, 2, 2, 2, 2, 2, 2, 2, 2, 2, 2, 1, 2, 2, 1, 1, 1, 1, 1, 2, 2, 1, 2, 2, 2, 2, 2, 2, 1, 1, 1, 2, 2, 1, 2, 2, 1, 2, 2, 1, 1, 1, 2, 2, 2, 2, 2, 1, 2, 2, 1, 1, 2, 2, 2, 2, 2, 1, 1, 1, 1, 1, 1, 1, 1, 1, 2, 2, 1, 2, 2, 2, 2, 2, 1, 1, 2, 2, 2, 1, 2, 2, 2, 2, 2, 2, 2, 4 ),
 ( 0.03433471828737562348, 0.03436343981862335223, 0.03439216134987107404, 0.03444960441236652460, 0.03456449053735742571, 0.03479426278733922795, 0.03525380728730283242, 0.03571335178726643689, 0.03594312403724823912, 0.03605801016223914024, 0.03608673169348686205, 0.03611545322473459080, 0.03617289628723004830, 0.03709198528715729193, 0.03755152978712091028, 0.03778130203710271945, 0.03783874509959817695, 0.03785310586522203785, 0.03786746663084590570, 0.03789618816209362751, 0.03801107428708454944, 0.03893016328701191797, 0.03938970778697560571, 0.03950459391196652764, 0.03956203697446198514, 0.03959075850570972083, 0.03960511927133358867, 0.03961948003695744958, 0.03984925228693930732, 0.04076834128686672443, 0.04122788578683042604, 0.04145765803681228379, 0.04168743028679414153, 0.04260651928672155864, 0.04306606378668526025, 0.04312350684918071775, 0.04318094991167618218, 0.04329583603666711106, 0.04352560828664896186, 0.04444469728657637897, 0.04467446953655822978, 0.04478935566154915865, 0.04484679872404462309, 0.04487552025529235183, 0.04488988102091621968, 0.04489347121232218490, 0.04489706140372815013, 0.04490424178654011528, 0.04536378628650494099, 0.04628287528643459242, 0.04651264753641700528, 0.04662753366140821171, 0.04665625519265600984, 0.04666343557546796805, 0.04667061595827991238, 0.04668497672390381492, 0.04674241978639941120, 0.04720196428636422303, 0.04812105328629383283, 0.04835082553627623181, 0.04840826859877183502, 0.04846571166126743824, 0.04858059778625863773, 0.04904014228622343569, 0.04995923128615303854, 0.05007411741114424497, 0.05013156047363984125, 0.05016028200488764632, 0.05017464277051153498, 0.05018900353613543752, 0.05041877578611784344, 0.05087832028608266222, 0.05179740928601228589, 0.05191229541100348538, 0.05192665617662738792, 0.05194101694225129046, 0.05196973847349908859, 0.05202718153599469181, 0.05225695378597709773, 0.05271649828594189569, 0.05363558728587150548, 0.05369303034836710176, 0.05372175187961490683, 0.05375047341086270497, 0.05386535953585390446, 0.05409513178583630344, 0.05455467628580110140, 0.05501422078576589242, 0.05524399303574828446, 0.05535887916073949089, 0.05541632222323508716, 0.05544504375448289224, 0.05545222413729483657, 0.05545940452010678090, 0.05547376528573066956, 0.05639285428565964098, 0.05685239878562411975, 0.05708217103560635913, 0.05719705716059747536, 0.05722577869184525962, 0.05725450022309304388, 0.05731194328558860546, 0.05823103228551756994, 0.05915012128544652747, 0.06006921028537549889, 0.06052875478533997766, 0.06064364091033110082, 0.06075852703532222399, 0.06098829928530446337, 0.06190738828523344173, 0.06236693278519793437, 0.06259670503518018070, 0.06282647728516242702, 0.06374556628509139844 ),
 .UNSPECIFIED. ) ;
#12345 = CARTESIAN_POINT ( 'NONE',  ( 11.71143458302510965, 54.18049042001842963, 6.715257056421563675 ) ) ;
#12346 = CARTESIAN_POINT ( 'NONE',  ( -10.26110598144033403, 64.59313657883589599, -8.772856892074198498 ) ) ;
#12347 = EDGE_LOOP ( 'NONE', ( #4728, #1333, #13825 ) ) ;
#12348 = CARTESIAN_POINT ( 'NONE',  ( -13.43241235626039831, 34.88232143987041667, -1.376510585871620229 ) ) ;
#12349 = ORIENTED_EDGE ( 'NONE', *, *, #17031, .F. ) ;
#12350 = CARTESIAN_POINT ( 'NONE',  ( 13.35186508744918576, 78.50178817042122148, -2.050551861675898646 ) ) ;
#12351 = CARTESIAN_POINT ( 'NONE',  ( 7.500000000000000888, 102.9299999999999073, 9.367496997597653419 ) ) ;
#12352 = CARTESIAN_POINT ( 'NONE',  ( 7.500000000000003553, -26.29769599445798534, 6.931232109908926908 ) ) ;
#12353 = CARTESIAN_POINT ( 'NONE',  ( 11.17057654354756657, 72.71510454181631644, -7.580829038184448088 ) ) ;
#12354 = CARTESIAN_POINT ( 'NONE',  ( 25.42428528562852819, 5.918584287042170544, 5.441113646577569796 ) ) ;
#12355 = CARTESIAN_POINT ( 'NONE',  ( -8.343458848123576743, -12.51999999999999780, -11.48378591275254301 ) ) ;
#12356 = CARTESIAN_POINT ( 'NONE',  ( 10.92172942406179104, 69.73000000000000398, -7.935100905948385908 ) ) ;
#12357 = CARTESIAN_POINT ( 'NONE',  ( -12.56842791742744758, 52.75088463843982822, -4.935720490616978928 ) ) ;
#12358 = CARTESIAN_POINT ( 'NONE',  ( -9.520470885617715595, 47.62999999999999545, -6.917026985038136289 ) ) ;
#12359 = CARTESIAN_POINT ( 'NONE',  ( 10.92172942406178926, 68.12999999999999545, 7.935100905948387684 ) ) ;
#12360 = CARTESIAN_POINT ( 'NONE',  ( -15.31996850146879652, 8.007813437504038845, -9.831838144771289478 ) ) ;
#12361 = CARTESIAN_POINT ( 'NONE',  ( 9.980839278485152732, 69.07821623398331212, 9.090265664844007887 ) ) ;
#12362 = CARTESIAN_POINT ( 'NONE',  ( -0.5739585204448709455, 37.20062488901800890, -13.49031863273558507 ) ) ;
#12363 = CARTESIAN_POINT ( 'NONE',  ( 1.900613283894434735, 4.622906826104707712, 12.00000000000000000 ) ) ;
#12364 = CARTESIAN_POINT ( 'NONE',  ( -13.16986379960055409, -17.65624999999997513, 13.16986379959834252 ) ) ;
#12365 = CARTESIAN_POINT ( 'NONE',  ( -6.131838958729160183, 74.45581572403800408, 12.02710268997748067 ) ) ;
#12366 = CARTESIAN_POINT ( 'NONE',  ( -13.36244170316012081, 76.86246845120821547, -1.928779065015713279 ) ) ;
#12367 = CARTESIAN_POINT ( 'NONE',  ( -8.343458848123582072, 0.3799999999999937317, 11.48378591275253768 ) ) ;
#12368 = CARTESIAN_POINT ( 'NONE',  ( -1.900613283894433181, 0.1229068261047050609, -12.00000000000000000 ) ) ;
#12369 = DIRECTION ( 'NONE',  ( 0.000000000000000000, 0.000000000000000000, -1.000000000000000000 ) ) ;
#12370 = CARTESIAN_POINT ( 'NONE',  ( -10.92172942406178926, 32.62999999999999545, -7.935100905948389460 ) ) ;
#12371 = CARTESIAN_POINT ( 'NONE',  ( -3.636496289402156190, -10.47000000000000064, 11.19198476289190758 ) ) ;
#12372 = EDGE_CURVE ( 'NONE', #13643, #7272, #9094, .T. ) ;
#12373 = CARTESIAN_POINT ( 'NONE',  ( 7.272992578804308828, 48.97999999999999687, 10.01041549318726886 ) ) ;
#12374 = CARTESIAN_POINT ( 'NONE',  ( 10.92172942406179104, -14.26999999999999780, -7.935100905948385908 ) ) ;
#12375 = CARTESIAN_POINT ( 'NONE',  ( -2.701716699869450178, 34.27714333493316445, -13.22690816007884784 ) ) ;
#12376 = CARTESIAN_POINT ( 'NONE',  ( 13.46309567844158117, 75.46468981469040216, -1.002245987159475549 ) ) ;
#12377 = CARTESIAN_POINT ( 'NONE',  ( 0.000000000000000000, 9.000000000000000000, 0.000000000000000000 ) ) ;
#12378 = VECTOR ( 'NONE', #1673, 1000.000000000000000 ) ;
#12379 = CARTESIAN_POINT ( 'NONE',  ( -7.272992578804310604, 33.38000000000000256, 10.01041549318726709 ) ) ;
#12380 = CARTESIAN_POINT ( 'NONE',  ( -11.21531812396516514, 41.21235424446476969, 7.514485397707633574 ) ) ;
#12381 = CARTESIAN_POINT ( 'NONE',  ( -0.5901369808829292074, 58.20121914870583169, -13.50000000000000178 ) ) ;
#12382 = CARTESIAN_POINT ( 'NONE',  ( -19.29752010712827826, 0.000000000000000000, -17.42428528562878398 ) ) ;
#12383 = CARTESIAN_POINT ( 'NONE',  ( 7.961489030491042840, 36.87882774062229174, -10.90288674562418869 ) ) ;
#12384 = CARTESIAN_POINT ( 'NONE',  ( 2.445080149700053643E-15, 4.180000000000004157, -13.50000000000000000 ) ) ;
#12385 = B_SPLINE_CURVE_WITH_KNOTS ( 'NONE', 3,
 ( #2214, #8969, #815, #17073, #15912, #16903, #14410, #8886, #4806, #7641, #17248, #989, #6226, #11612, #3731, #14496, #4977, #15734, #15562, #899, #11784, #3643, #6490, #14241, #16988, #7726, #10293, #15645, #5161, #9057, #2298, #10553, #17160, #5072, #7819, #10466, #15827, #2126, #13191, #12931, #7552, #1076, #3821, #9235, #14589, #7469, #12849, #738, #15998, #12039, #12, #13614, #1246, #10718, #1165, #194, #1327, #6576, #14755, #8161, #10981, #1507, #3903, #13357, #2733, #17418, #5333, #6923, #16083, #6658, #12300, #2644, #3991, #16260, #9407, #8076, #9321, #10805, #7989, #14671, #13440, #2559, #1415, #14839, #6743, #6833, #11957, #12123, #5416, #16167, #5599, #4077, #9492, #17336, #16351, #10633, #13526, #12209, #103, #5508, #10891, #2822, #4167, #4257, #9579, #7902, #2469, #14930, #8252, #9667, #13277, #5247, #3090, #12565, #7094, #11418, #12478, #11326, #8516, #4696, #7263, #2909, #13695, #11240, #7011, #12388, #15017, #536, #4436, #8339, #279, #16790, #13953, #1594, #5946, #5688, #16704, #11068, #8687, #13779, #6035, #364, #13866, #7357, #1768, #16441, #4343, #3270, #9752, #15097, #2996, #8426, #1678, #5769, #11153, #16529, #624, #9843, #15189, #1850, #7177, #14046, #451, #12647, #5861, #16618, #4522, #9929, #4609, #10016, #15278, #1934, #3179, #8601, #15364, #12736, #14303, #13168, #17051, #17226, #10444, #9033, #15538, #10101, #15622, #6288, #15452, #8777, #11675, #2020, #7446, #3361, #13079 ),
 .UNSPECIFIED., .F., .F.,
 ( 4, 2, 2, 1, 2, 2, 1, 1, 1, 2, 2, 1, 2, 2, 1, 1, 2, 2, 2, 2, 2, 1, 1, 2, 2, 2, 2, 2, 2, 1, 1, 2, 2, 1, 1, 1, 2, 2, 1, 2, 2, 2, 2, 2, 1, 1, 2, 2, 2, 1, 2, 2, 1, 1, 2, 2, 2, 2, 2, 1, 2, 2, 2, 1, 2, 2, 1, 2, 2, 2, 2, 2, 2, 1, 2, 2, 2, 2, 2, 1, 1, 1, 1, 2, 1, 1, 1, 2, 2, 1, 1, 2, 2, 2, 2, 2, 2, 1, 1, 2, 2, 2, 1, 2, 2, 1, 2, 2, 2, 2, 2, 1, 1, 2, 2, 4 ),
 ( 0.3284481763819381284, 0.3293659151444585653, 0.3302836539069789468, 0.3303410125796364949, 0.3303553522478008819, 0.3303696919159652690, 0.3303983712522940430, 0.3305130885976090838, 0.3307425232882391652, 0.3312013926694993837, 0.3321191314320198207, 0.3322338487773348614, 0.3322625281136636355, 0.3322768677818280225, 0.3322912074499924096, 0.3323485661226499022, 0.3325780008132800947, 0.3330368701945404797, 0.3339546089570611942, 0.3341840436476913867, 0.3342127229840201608, 0.3342414023203489348, 0.3342987609930064830, 0.3344134783383215792, 0.3348723477195819642, 0.3357900864821026787, 0.3360195211727328712, 0.3360768798453904194, 0.3361055591817191934, 0.3361342385180479675, 0.3362489558633630637, 0.3367078252446234488, 0.3376255640071442743, 0.3378549986977744668, 0.3379697160430895631, 0.3379983953794183371, 0.3380055652135005584, 0.3380127350475827241, 0.3380270747157471112, 0.3380844333884046593, 0.3385433027696648223, 0.3394610415321852592, 0.3399199109134454777, 0.3399772695861030258, 0.3400346282587605184, 0.3401493456040756147, 0.3403787802947056962, 0.3412965190572261331, 0.3417553884384863516, 0.3418127471111438997, 0.3418270867793082868, 0.3418414264474726183, 0.3418701057838013924, 0.3419848231291164331, 0.3422142578197465146, 0.3431319965822668405, 0.3435908659635270590, 0.3437055833088420997, 0.3437629419814995924, 0.3438203006541571405, 0.3440497353447872220, 0.3449674741073075479, 0.3458852128698278738, 0.3459425715424854220, 0.3459712508788141960, 0.3459999302151429146, 0.3461146475604579553, 0.3463440822510880923, 0.3468029516323482553, 0.3477206903948685812, 0.3481795597761287442, 0.3482082391124575182, 0.3482369184487862923, 0.3482942771214438404, 0.3484089944667588812, 0.3486384291573890182, 0.3490972985386492922, 0.3493267332292794292, 0.3493410728974438162, 0.3493554125656082032, 0.3493840919019369773, 0.3494414505745945254, 0.3495561679199096772, 0.3500150373011700622, 0.3502444719918003102, 0.3503591893371154065, 0.3504165480097729546, 0.3504452273461017286, 0.3504523971801839499, 0.3504595670142661157, 0.3504739066824305027, 0.3513916454449503290, 0.3523093842074701554, 0.3525388188981000703, 0.3526535362434150556, 0.3526678759115794426, 0.3526822155797438296, 0.3527108949160725482, 0.3527682535887300408, 0.3532271229699898707, 0.3541448617325096415, 0.3559803392575490721, 0.3560090185938777907, 0.3560233582620421777, 0.3560376979302065648, 0.3560950566028640019, 0.3562097739481789871, 0.3564392086388087910, 0.3568980780200685099, 0.3573569474013282288, 0.3575863820919580882, 0.3576437407646155808, 0.3576724201009442994, 0.3576867597691086309, 0.3577010994372730179, 0.3578158167825879477 ),
 .UNSPECIFIED. ) ;
#12386 = CARTESIAN_POINT ( 'NONE',  ( 0.000000000000000000, 80.93000000000000682, 0.000000000000000000 ) ) ;
#12387 = CARTESIAN_POINT ( 'NONE',  ( -4.816349661276159821, 49.35356466364647332, -12.61319266799936223 ) ) ;
#12388 = CARTESIAN_POINT ( 'NONE',  ( 11.49974279481918948, 63.16598485185204481, 7.071657227356595854 ) ) ;
#12389 = CARTESIAN_POINT ( 'NONE',  ( 8.386380085766983683, 42.00036598867336579, 10.57921543981575851 ) ) ;
#12390 = CARTESIAN_POINT ( 'NONE',  ( 0.8900221435513422374, 38.71200720458531919, 13.47797817745645865 ) ) ;
#12391 = AXIS2_PLACEMENT_3D ( 'NONE', #1008, #8900, #14427 ) ;
#12392 = VERTEX_POINT ( 'NONE', #976 ) ;
#12393 = CARTESIAN_POINT ( 'NONE',  ( 9.520470885617715595, 76.13000000000000966, 6.917026985038134512 ) ) ;
#12394 = CARTESIAN_POINT ( 'NONE',  ( -9.708203932499371192, 4.096025403784449459, 7.053423027509678533 ) ) ;
#12395 = CARTESIAN_POINT ( 'NONE',  ( 9.538709233711902776E-13, -20.81249999999995026, -11.37500000000000000 ) ) ;
#12396 = CARTESIAN_POINT ( 'NONE',  ( -10.92172942406178926, 7.629999999999998117, -7.935100905948389460 ) ) ;
#12397 = ORIENTED_EDGE ( 'NONE', *, *, #10372, .F. ) ;
#12398 = EDGE_CURVE ( 'NONE', #12392, #39, #5059, .T. ) ;
#12399 = CARTESIAN_POINT ( 'NONE',  ( -2.284164177028834342, 43.26213011653167939, -13.30536795550864149 ) ) ;
#12400 = CARTESIAN_POINT ( 'NONE',  ( -7.499999999999998224, 108.6199039925686662, 2.572187159835563897 ) ) ;
#12401 = CARTESIAN_POINT ( 'NONE',  ( 11.56739400518585192, 60.68949195955414666, -6.960273062025671642 ) ) ;
#12402 = CARTESIAN_POINT ( 'NONE',  ( 13.50000000000000000, -1.569999999999994955, 1.734723475976807094E-15 ) ) ;
#12403 = CARTESIAN_POINT ( 'NONE',  ( 0.000000000000000000, 0.000000000000000000, 9.500000000000021316 ) ) ;
#12404 = CARTESIAN_POINT ( 'NONE',  ( 13.42937308305210919, 66.38180020187820674, 1.390829281587693478 ) ) ;
#12405 = CARTESIAN_POINT ( 'NONE',  ( 1.463318478726158389, 56.73261554528513528, 13.42046002623553669 ) ) ;
#12406 = CARTESIAN_POINT ( 'NONE',  ( -7.272992578804307939, 59.48000000000000398, -10.01041549318726886 ) ) ;
#12407 = CARTESIAN_POINT ( 'NONE',  ( 11.76794919243112325, 67.43000000000000682, 1.441158131103945434E-15 ) ) ;
#12408 = CARTESIAN_POINT ( 'NONE',  ( -12.95528734819502503, 47.06741981842274924, 3.836386419411801807 ) ) ;
#12409 = AXIS2_PLACEMENT_3D ( 'NONE', #4012, #3924, #6943 ) ;
#12410 = CARTESIAN_POINT ( 'NONE',  ( -13.49999999999999822, 46.07999999999999829, 4.386415899144235020 ) ) ;
#12411 = CYLINDRICAL_SURFACE ( 'NONE', #15296, 13.50000000000000000 ) ;
#12412 = CARTESIAN_POINT ( 'NONE',  ( 9.037365757593402549, 30.82912645640030647, -10.03076112684414589 ) ) ;
#12413 = CARTESIAN_POINT ( 'NONE',  ( -5.572576793242300042, 56.47777282521396813, 12.29619502175249401 ) ) ;
#12414 = CARTESIAN_POINT ( 'NONE',  ( 9.538709233711902776E-13, -70.76249999999983231, -11.37500000000000000 ) ) ;
#12415 = CARTESIAN_POINT ( 'NONE',  ( 13.50000000000000000, 6.430000000000005045, 1.734723475976807094E-15 ) ) ;
#12416 = CARTESIAN_POINT ( 'NONE',  ( 1.324280721486043255, 32.72761620803525062, 13.43490005586108360 ) ) ;
#12417 = CARTESIAN_POINT ( 'NONE',  ( 4.935098408141093351, 10.00000000000000000, 12.34347594669868720 ) ) ;
#12418 = CARTESIAN_POINT ( 'NONE',  ( 3.652837425045026176, 40.04880968999665214, -13.00149846498695005 ) ) ;
#12419 = CARTESIAN_POINT ( 'NONE',  ( -7.409984580736203970E-16, 22.68000000000000327, 12.37355403259654985 ) ) ;
#12420 = ORIENTED_EDGE ( 'NONE', *, *, #13794, .F. ) ;
#12421 = CARTESIAN_POINT ( 'NONE',  ( -2.064298368984843535, 62.60577758412497218, 13.34129268682456981 ) ) ;
#12422 = EDGE_LOOP ( 'NONE', ( #15785, #9173 ) ) ;
#12423 = EDGE_CURVE ( 'NONE', #3781, #17339, #1929, .T. ) ;
#12424 = CARTESIAN_POINT ( 'NONE',  ( -7.272992578804310604, -16.62000000000000099, 10.01041549318726709 ) ) ;
#12425 = CARTESIAN_POINT ( 'NONE',  ( 1.561832610794586740E-12, -61.36249999999986215, -18.62500000000000000 ) ) ;
#12426 = CARTESIAN_POINT ( 'NONE',  ( -11.19741182518031053, 44.21346306567002671, 7.541088250378106039 ) ) ;
#12427 = CARTESIAN_POINT ( 'NONE',  ( 10.92172942406178926, 65.12999999999999545, 7.935100905948387684 ) ) ;
#12428 = CARTESIAN_POINT ( 'NONE',  ( -4.171729424061791036, 32.52999999999999403, 12.83926296998457239 ) ) ;
#12429 = CARTESIAN_POINT ( 'NONE',  ( -8.691771469529815392E-16, 43.67999999999998550, 14.19474002721660355 ) ) ;
#12430 = CARTESIAN_POINT ( 'NONE',  ( -6.327032371063140204, 46.41202214260281522, -11.92554859961118119 ) ) ;
#12431 = CARTESIAN_POINT ( 'NONE',  ( -3.712474928015834230, 67.31306499987073266, -12.98134956584450350 ) ) ;
#12432 = CARTESIAN_POINT ( 'NONE',  ( 18.62500000000000000, -92.64999999999974989, 1.560692158462880521E-12 ) ) ;
#12433 =( BOUNDED_CURVE ( )  B_SPLINE_CURVE ( 2, ( #17156, #4973, #10376, #10462, #15822, #15908, #17245, #10549, #3817, #14584, #2465, #7897, #13273 ),
 .UNSPECIFIED., .F., .F. ) 
 B_SPLINE_CURVE_WITH_KNOTS ( ( 3, 2, 2, 2, 2, 2, 3 ),
 ( 0.3194444444444444198, 0.3222222222222222432, 0.3277777777777777790, 0.3333333333333333148, 0.3388888888888889062, 0.3444444444444444420, 0.3472222222222222099 ),
 .UNSPECIFIED. ) 
 CURVE ( )  GEOMETRIC_REPRESENTATION_ITEM ( )  RATIONAL_B_SPLINE_CURVE ( ( 0.9755282581475768211, 0.9755282581475765991, 1.000000000000000000, 0.9510565162951535312, 1.000000000000000000, 0.9510565162951535312, 1.000000000000000000, 0.9510565162951535312, 1.000000000000000000, 0.9510565162951535312, 1.000000000000000000, 0.9755282581475768211, 0.9755282581475768211 ) ) 
 REPRESENTATION_ITEM ( '' )  );
#12434 = CARTESIAN_POINT ( 'NONE',  ( 12.95352307866690111, 54.56613520967127329, -3.803420169897604008 ) ) ;
#12435 = CARTESIAN_POINT ( 'NONE',  ( -5.827146427730992784, 64.39213759910121837, -12.17765789728212766 ) ) ;
#12436 = EDGE_LOOP ( 'NONE', ( #13199, #8015, #11618, #12781 ) ) ;
#12437 = CARTESIAN_POINT ( 'NONE',  ( -8.891200544363830713E-16, 64.67999999999999261, 13.50000000000000000 ) ) ;
#12438 = CARTESIAN_POINT ( 'NONE',  ( -13.49990086529558830, 34.94504141492947724, 0.4412720814781904144 ) ) ;
#12439 = ORIENTED_EDGE ( 'NONE', *, *, #10408, .T. ) ;
#12440 = CARTESIAN_POINT ( 'NONE',  ( 13.46864404905786117, 78.46180393935253505, -0.9198462106560619800 ) ) ;
#12441 = CARTESIAN_POINT ( 'NONE',  ( -25.42428528562860279, 0.000000000000000000, 5.441113646577211860 ) ) ;
#12442 = VECTOR ( 'NONE', #10051, 1000.000000000000114 ) ;
#12443 = CARTESIAN_POINT ( 'NONE',  ( 7.500000000000001776, -27.68990399256866652, 2.572187159835578552 ) ) ;
#12444 = CARTESIAN_POINT ( 'NONE',  ( 8.010861774722636497, 72.87662127041942028, -10.86656001248561587 ) ) ;
#12445 = CARTESIAN_POINT ( 'NONE',  ( 1.758123048363891883, 79.11681026432344765, -13.38681728492156431 ) ) ;
#12446 = CARTESIAN_POINT ( 'NONE',  ( -13.50000000000000000, -15.07000000000000028, -3.469446951953614189E-15 ) ) ;
#12447 = CARTESIAN_POINT ( 'NONE',  ( 10.92172942406178926, 66.12999999999999545, 7.935100905948387684 ) ) ;
#12448 = CARTESIAN_POINT ( 'NONE',  ( -13.20937656505621227, 53.02849338733904716, 2.786178234548895905 ) ) ;
#12449 = CARTESIAN_POINT ( 'NONE',  ( 9.520470885617715595, 40.12999999999999545, 6.917026985038134512 ) ) ;
#12450 = CARTESIAN_POINT ( 'NONE',  ( -3.636496289402152637, -17.66999999999999815, -11.19198476289190936 ) ) ;
#12451 = CARTESIAN_POINT ( 'NONE',  ( -10.92172942406179104, 61.22999999999999687, 7.935100905948387684 ) ) ;
#12452 = CARTESIAN_POINT ( 'NONE',  ( -7.499999999999996447, 88.93000000000000682, -12.00000000000000178 ) ) ;
#12453 = ADVANCED_FACE ( 'NONE', ( #2723 ), #9136, .T. ) ;
#12454 = CARTESIAN_POINT ( 'NONE',  ( 5.752805971757215531, 68.88911494562405835, 12.22037727962858611 ) ) ;
#12455 = CARTESIAN_POINT ( 'NONE',  ( 0.000000000000000000, 0.000000000000000000, 0.000000000000000000 ) ) ;
#12456 = CARTESIAN_POINT ( 'NONE',  ( 1.948779282392957057, 35.75006106732994482, 13.35913770969951564 ) ) ;
#12457 = CARTESIAN_POINT ( 'NONE',  ( -13.16986379959834252, -80.09374999999982947, -13.16986379960055409 ) ) ;
#12458 = CARTESIAN_POINT ( 'NONE',  ( -10.46266594696475316, 74.25595380999331496, 8.531279792551288210 ) ) ;
#12459 = CARTESIAN_POINT ( 'NONE',  ( -4.671281222091343999, 76.34819209519075400, -12.66606340400099562 ) ) ;
#12460 = LINE ( 'NONE', #12631, #11841 ) ;
#12461 = DIRECTION ( 'NONE',  ( -0.000000000000000000, 1.000000000000000000, -0.000000000000000000 ) ) ;
#12462 = CARTESIAN_POINT ( 'NONE',  ( -11.52888015854957793, 80.93000000000003524, 3.329402692645399675 ) ) ;
#12463 = CARTESIAN_POINT ( 'NONE',  ( -8.549982208541774191E-16, 30.68000000000001037, 14.19474002721660355 ) ) ;
#12464 = CARTESIAN_POINT ( 'NONE',  ( -3.636496289402156190, -7.469999999999997087, 11.19198476289190758 ) ) ;
#12465 = CARTESIAN_POINT ( 'NONE',  ( -11.76794919243112325, 35.92999999999999972, -2.882316262207890869E-15 ) ) ;
#12466 = CARTESIAN_POINT ( 'NONE',  ( -17.32050807568884210, 0.000000000000000000, 7.999999999999840128 ) ) ;
#12467 = CARTESIAN_POINT ( 'NONE',  ( -9.257301361965243558, 32.31846096236034782, 9.826932714272743397 ) ) ;
#12468 = CARTESIAN_POINT ( 'NONE',  ( 12.22812538439530528, 75.22023328956014154, 5.720436177748926987 ) ) ;
#12469 = CARTESIAN_POINT ( 'NONE',  ( 9.651058002246328371, 3.646912567499685897E-17, -14.62992131181279021 ) ) ;
#12470 = CARTESIAN_POINT ( 'NONE',  ( -11.76794919243112325, 33.07999999999998408, 3.823638476888994386 ) ) ;
#12471 = CARTESIAN_POINT ( 'NONE',  ( 4.558948942910276969, 52.01595162841300635, -12.70712274664167474 ) ) ;
#12472 = ADVANCED_FACE ( 'NONE', ( #4068 ), #7807, .F. ) ;
#12473 = CARTESIAN_POINT ( 'NONE',  ( 2.445080149700053643E-15, 1.180000000000002602, -13.50000000000000000 ) ) ;
#12474 = CARTESIAN_POINT ( 'NONE',  ( 0.1004344462107467778, 37.17638874791335013, -13.49962723151365296 ) ) ;
#12475 = CARTESIAN_POINT ( 'NONE',  ( -7.291143994141260196E-08, 47.67999796853253258, 13.49999999999999822 ) ) ;
#12476 = CARTESIAN_POINT ( 'NONE',  ( 12.50000000000000000, -18.00000000000000355, -9.000000000000001776 ) ) ;
#12477 = AXIS2_PLACEMENT_3D ( 'NONE', #10344, #7950, #864 ) ;
#12478 = CARTESIAN_POINT ( 'NONE',  ( 11.73819402979808046, 63.18233018420252023, 6.670510071192460089 ) ) ;
#12479 = CARTESIAN_POINT ( 'NONE',  ( 13.44060992811053623, 42.38566405594722397, 1.278966233340825154 ) ) ;
#12480 = CARTESIAN_POINT ( 'NONE',  ( -18.35881383260822020, 7.956441918454669526, -1.156263389813576792 ) ) ;
#12481 = CARTESIAN_POINT ( 'NONE',  ( -11.76794919243112325, 24.78000000000000824, -3.823638476888998827 ) ) ;
#12482 = EDGE_LOOP ( 'NONE', ( #2868, #6864 ) ) ;
#12483 = CARTESIAN_POINT ( 'NONE',  ( 11.76794919243112325, 76.42999999999999261, 1.441158131103945434E-15 ) ) ;
#12484 = CARTESIAN_POINT ( 'NONE',  ( 2.222800136090958073E-15, 0.04602540378443767399, -12.00000000000000000 ) ) ;
#12485 = CARTESIAN_POINT ( 'NONE',  ( 4.711679271994910323, -69.72187499999984084, -11.37499999999960387 ) ) ;
#12486 = CARTESIAN_POINT ( 'NONE',  ( -4.171729424061787483, 4.330000000000000071, -12.83926296998457417 ) ) ;
#12487 = ORIENTED_EDGE ( 'NONE', *, *, #7738, .F. ) ;
#12488 = CARTESIAN_POINT ( 'NONE',  ( -9.800337745008080859, 43.56848657308245976, -9.294634735303336726 ) ) ;
#12489 = CARTESIAN_POINT ( 'NONE',  ( -7.499999999999998224, 108.7258046340737963, 1.043242051446487517 ) ) ;
#12490 = CARTESIAN_POINT ( 'NONE',  ( 9.464546292035263875, 60.80808485042920353, -9.627110977571010864 ) ) ;
#12491 = CARTESIAN_POINT ( 'NONE',  ( -4.171729424061791036, 6.530000000000008242, 12.83926296998457239 ) ) ;
#12492 = CARTESIAN_POINT ( 'NONE',  ( -7.714727599197334307, -5.203124999999987566, -18.62500000000064304 ) ) ;
#12493 = CARTESIAN_POINT ( 'NONE',  ( 10.07262787396443748, 66.08313066052312479, 8.989075947907759101 ) ) ;
#12494 = CARTESIAN_POINT ( 'NONE',  ( 8.577460307545479168, 57.00915232730558557, 10.42567900465104280 ) ) ;
#12495 = CARTESIAN_POINT ( 'NONE',  ( 11.76794919243112325, 58.28000000000000114, 3.823638476888996607 ) ) ;
#12496 = CARTESIAN_POINT ( 'NONE',  ( 10.92172942406178926, 35.13000000000000256, 7.935100905948387684 ) ) ;
#12497 = CARTESIAN_POINT ( 'NONE',  ( 7.272992578804308828, 66.98000000000000398, 10.01041549318726709 ) ) ;
#12498 = AXIS2_PLACEMENT_3D ( 'NONE', #12386, #276, #12207 ) ;
#12499 = CARTESIAN_POINT ( 'NONE',  ( -12.57615766451182537, 46.75189198415294101, -4.908197936080784807 ) ) ;
#12500 = CARTESIAN_POINT ( 'NONE',  ( 11.82910594196685850, 45.67102758238960547, -6.505590469736891812 ) ) ;
#12501 = CARTESIAN_POINT ( 'NONE',  ( 0.000000000000000000, 5.918584287042170544, 0.000000000000000000 ) ) ;
#12502 = ADVANCED_FACE ( 'NONE', ( #14746 ), #2372, .T. ) ;
#12503 = CARTESIAN_POINT ( 'NONE',  ( 2.919510057594956187, 31.07524303651355169, -13.20096495093523004 ) ) ;
#12504 = CARTESIAN_POINT ( 'NONE',  ( -11.03450900954605629, 9.999999999999994671, -5.378144140920507965 ) ) ;
#12505 = CARTESIAN_POINT ( 'NONE',  ( -4.711679271993004292, -88.45312499999978684, -11.37500000000039435 ) ) ;
#12506 = LINE ( 'NONE', #5354, #5853 ) ;
#12507 = CARTESIAN_POINT ( 'NONE',  ( 0.2224977522097629223, 32.68807153545635913, 13.49999999993604760 ) ) ;
#12508 = CARTESIAN_POINT ( 'NONE',  ( -1.844924112955495524E-14, 72.18000000000000682, -13.50000000000000000 ) ) ;
#12509 = CARTESIAN_POINT ( 'NONE',  ( -8.393536083122315361, 8.020663292675294542, -16.10013384871447073 ) ) ;
#12510 = ORIENTED_EDGE ( 'NONE', *, *, #8935, .T. ) ;
#12511 = CARTESIAN_POINT ( 'NONE',  ( -13.46962982805347231, 61.96129992434394040, 0.9054387881791874371 ) ) ;
#12512 = ORIENTED_EDGE ( 'NONE', *, *, #16969, .T. ) ;
#12513 = AXIS2_PLACEMENT_3D ( 'NONE', #14286, #10252, #3159 ) ;
#12514 = CARTESIAN_POINT ( 'NONE',  ( -11.76794919243112325, -17.22000000000000597, -3.823638476888998827 ) ) ;
#12515 = CARTESIAN_POINT ( 'NONE',  ( -13.16986379960055409, -67.60624999999984652, 13.16986379959834252 ) ) ;
#12516 = CARTESIAN_POINT ( 'NONE',  ( -12.80129509359390738, 43.77561004955722268, -4.287691323260377274 ) ) ;
#12517 = CARTESIAN_POINT ( 'NONE',  ( -9.314791131849382566, 8.055324194567102580, 15.43323788540787866 ) ) ;
#12518 = CARTESIAN_POINT ( 'NONE',  ( -13.49999999999999822, 38.07999999999999829, 4.386415899144235908 ) ) ;
#12519 = CARTESIAN_POINT ( 'NONE',  ( -10.92172942406179104, 46.22999999999999687, 7.935100905948387684 ) ) ;
#12520 = EDGE_CURVE ( 'NONE', #717, #10228, #3649, .T. ) ;
#12521 = CARTESIAN_POINT ( 'NONE',  ( -5.471725549333255501, 46.37816455119584447, -12.34359373141929872 ) ) ;
#12522 = CARTESIAN_POINT ( 'NONE',  ( -5.584685134716633748, 67.38269536530388848, -12.29070702121700620 ) ) ;
#12523 = CARTESIAN_POINT ( 'NONE',  ( -18.62499999999935341, -49.98437499999987210, -7.714727599200458030 ) ) ;
#12524 = CARTESIAN_POINT ( 'NONE',  ( 3.294022803995052762, 53.79842651621079597, 13.09196167790783605 ) ) ;
#12525 = CARTESIAN_POINT ( 'NONE',  ( -3.061294706506703545, 64.29016813706658695, -13.14846668619222392 ) ) ;
#12526 = ORIENTED_EDGE ( 'NONE', *, *, #13910, .T. ) ;
#12527 = CARTESIAN_POINT ( 'NONE',  ( -5.592873841450387573, 34.38301124043937307, -12.28706942924041989 ) ) ;
#12528 = CARTESIAN_POINT ( 'NONE',  ( 11.37500000000039435, -67.64062499999984368, -4.711679271993004292 ) ) ;
#12529 = CARTESIAN_POINT ( 'NONE',  ( 10.68121621590718995, 78.11601607104590528, 8.257274610802166848 ) ) ;
#12530 = CARTESIAN_POINT ( 'NONE',  ( -15.50190989971486921, 7.815224736851130949, 10.85009556066079917 ) ) ;
#12531 = CARTESIAN_POINT ( 'NONE',  ( 7.500000000000000888, -27.80979767490545029, -0.4943161440816083441 ) ) ;
#12532 = CARTESIAN_POINT ( 'NONE',  ( 12.57737074227892826, 72.25174867838231307, 4.912843465583652147 ) ) ;
#12533 = CARTESIAN_POINT ( 'NONE',  ( -8.549982208541774191E-16, -11.32000000000000028, 14.19474002721660355 ) ) ;
#12534 = CARTESIAN_POINT ( 'NONE',  ( -8.343458848123576743, 58.47999999999998977, -11.48378591275254301 ) ) ;
#12535 = CARTESIAN_POINT ( 'NONE',  ( -13.19435882288848028, 53.03109597840953171, 2.856512463374823341 ) ) ;
#12536 = CARTESIAN_POINT ( 'NONE',  ( 7.272992578804308828, 36.97999999999998977, 10.01041549318726709 ) ) ;
#12537 = CARTESIAN_POINT ( 'NONE',  ( -11.76794919243112325, -17.06999999999999318, -2.602085213965210642E-15 ) ) ;
#12538 = CARTESIAN_POINT ( 'NONE',  ( 10.92172942406178926, 56.13000000000000256, 7.935100905948387684 ) ) ;
#12539 = CARTESIAN_POINT ( 'NONE',  ( 4.171729424061791924, 78.03000000000000114, -12.83926296998457239 ) ) ;
#12540 = CARTESIAN_POINT ( 'NONE',  ( 3.636496289402157078, -2.970000000000000639, -11.19198476289190936 ) ) ;
#12541 = CARTESIAN_POINT ( 'NONE',  ( 3.562763415993998262, 68.80810093510450542, 13.02139636752514207 ) ) ;
#12542 = CARTESIAN_POINT ( 'NONE',  ( -3.048821793079171893, 37.28962259733035012, -13.15181977963969651 ) ) ;
#12543 = CARTESIAN_POINT ( 'NONE',  ( -2.138189944381247098, 72.25688142232026223, -13.49999999999999645 ) ) ;
#12544 = CARTESIAN_POINT ( 'NONE',  ( -18.62500000000000000, -65.52499999999986358, -1.562973063126292757E-12 ) ) ;
#12545 = CARTESIAN_POINT ( 'NONE',  ( -11.59403592772097547, 73.67225474520861894, -6.918110984581458567 ) ) ;
#12546 = CARTESIAN_POINT ( 'NONE',  ( -8.762708921790252958, 76.51760276393278559, -10.27614992352630274 ) ) ;
#12547 = CARTESIAN_POINT ( 'NONE',  ( 19.79706521687762688, 7.170682760640494813, 8.000000000000092371 ) ) ;
#12548 = DIRECTION ( 'NONE',  ( -0.000000000000000000, -1.000000000000000000, -0.000000000000000000 ) ) ;
#12549 = CYLINDRICAL_SURFACE ( 'NONE', #12797, 13.50000000000000000 ) ;
#12550 = CARTESIAN_POINT ( 'NONE',  ( -4.171729424061787483, 32.32999999999999829, -12.83926296998457417 ) ) ;
#12551 = CARTESIAN_POINT ( 'NONE',  ( 7.272992578804308828, -7.020000000000005791, 10.01041549318726709 ) ) ;
#12552 = CARTESIAN_POINT ( 'NONE',  ( -11.76794919243112325, 35.77999999999999403, -3.823638476888998827 ) ) ;
#12553 = CARTESIAN_POINT ( 'NONE',  ( 4.171729424061789260, -15.16999999999999638, 12.83926296998457239 ) ) ;
#12554 = CARTESIAN_POINT ( 'NONE',  ( 1.628308837847167748E-06, 32.68004529479373588, 13.49999999999980460 ) ) ;
#12555 = CARTESIAN_POINT ( 'NONE',  ( 13.47305538128101077, 75.45974515404770955, -0.8610043160690442621 ) ) ;
#12556 = ADVANCED_FACE ( 'NONE', ( #2458 ), #1153, .F. ) ;
#12557 = CARTESIAN_POINT ( 'NONE',  ( 8.834039747090045580, 3.646912567496566199E-17, -14.96760085455396805 ) ) ;
#12558 = CARTESIAN_POINT ( 'NONE',  ( 11.76794919243112680, 34.57999999999999829, -3.823638476888993942 ) ) ;
#12559 = CARTESIAN_POINT ( 'NONE',  ( 8.050218389484046000, 31.03187319105529340, 8.940655939244130934 ) ) ;
#12560 = CARTESIAN_POINT ( 'NONE',  ( 10.14124484132416626, 51.77333499035184872, -8.911260184641234261 ) ) ;
#12561 = DIRECTION ( 'NONE',  ( 0.000000000000000000, 0.000000000000000000, 1.000000000000000000 ) ) ;
#12562 = CARTESIAN_POINT ( 'NONE',  ( 8.267901496158602370, 36.86504151979552546, -10.67201748973769782 ) ) ;
#12563 = PLANE ( 'NONE',  #2864 ) ;
#12564 = CARTESIAN_POINT ( 'NONE',  ( -0.3617901473021373771, 49.19299986674817404, -13.49533619113506688 ) ) ;
#12565 = CARTESIAN_POINT ( 'NONE',  ( 12.47474062557478192, 63.24199196955865432, 5.166233987108326708 ) ) ;
#12566 = CARTESIAN_POINT ( 'NONE',  ( 10.89469735476495416, 42.12845549515284205, 7.973421550594564700 ) ) ;
#12567 = CARTESIAN_POINT ( 'NONE',  ( 10.70081124441169784, 48.74267151870439108, -8.230608850174302660 ) ) ;
#12568 = CARTESIAN_POINT ( 'NONE',  ( -7.272992578804310604, 22.38000000000000966, 10.01041549318726709 ) ) ;
#12569 = VERTEX_POINT ( 'NONE', #6648 ) ;
#12570 = CARTESIAN_POINT ( 'NONE',  ( 11.76794919243112680, 67.57999999999998408, -3.823638476888993942 ) ) ;
#12571 = CARTESIAN_POINT ( 'NONE',  ( -18.62499999999935341, -83.28437499999976978, -7.714727599200458030 ) ) ;
#12572 = CARTESIAN_POINT ( 'NONE',  ( -11.37500000000000000, -24.97499999999994102, -9.545674412382054647E-13 ) ) ;
#12573 = CARTESIAN_POINT ( 'NONE',  ( -8.343458848123576743, 7.480000000000002203, -11.48378591275254301 ) ) ;
#12574 = VERTEX_POINT ( 'NONE', #17409 ) ;
#12575 = CARTESIAN_POINT ( 'NONE',  ( -9.182998036710223744, 43.53789999169043057, -9.897881256833889196 ) ) ;
#12576 = CARTESIAN_POINT ( 'NONE',  ( 1.775737858763662015E-15, 9.999999999999998224, 14.50000000000000000 ) ) ;
#12577 = CARTESIAN_POINT ( 'NONE',  ( -8.343458848123576743, -0.5200000000000069011, -11.48378591275254301 ) ) ;
#12578 = CARTESIAN_POINT ( 'NONE',  ( -9.708203932499369415, 6.496025403784435603, -7.053423027509682086 ) ) ;
#12579 = CARTESIAN_POINT ( 'NONE',  ( 8.206140411365607790, 65.99215479700292519, 10.71966715772747669 ) ) ;
#12580 = CARTESIAN_POINT ( 'NONE',  ( 1.580573102785959083, 56.73683176799062267, 13.40744280352419437 ) ) ;
#12581 = CARTESIAN_POINT ( 'NONE',  ( 11.76794919243112680, 58.57999999999999119, -3.823638476888993942 ) ) ;
#12582 = CARTESIAN_POINT ( 'NONE',  ( -11.76794919243112325, 65.93000000000000682, -2.882316262207890869E-15 ) ) ;
#12583 = CARTESIAN_POINT ( 'NONE',  ( -13.49125618869725862, 46.94671107676184363, 0.4858370549406775818 ) ) ;
#12584 = CARTESIAN_POINT ( 'NONE',  ( 6.997088715578399842, 45.92049188004365590, -11.54634344188570161 ) ) ;
#12585 = LINE ( 'NONE', #7285, #9114 ) ;
#12586 = CARTESIAN_POINT ( 'NONE',  ( 8.352825653922046456, 30.86116902798444173, -10.60567559741120469 ) ) ;
#12587 = CARTESIAN_POINT ( 'NONE',  ( -4.507315936713728988, 56.51790915384739833, 12.73940224085357009 ) ) ;
#12588 = CARTESIAN_POINT ( 'NONE',  ( 4.171729424061789260, 52.83000000000000540, 12.83926296998457417 ) ) ;
#12589 = CARTESIAN_POINT ( 'NONE',  ( 3.595939032899281074, 32.80928899092024409, 13.01768941633015686 ) ) ;
#12590 = CARTESIAN_POINT ( 'NONE',  ( -2.219840399520819574, 10.00000000000000711, 12.61519577489909949 ) ) ;
#12591 = CYLINDRICAL_SURFACE ( 'NONE', #6634, 26.00000000000000355 ) ;
#12592 = VERTEX_POINT ( 'NONE', #8066 ) ;
#12593 = CARTESIAN_POINT ( 'NONE',  ( -8.680814540994266082, 62.34599070752307171, 10.33893831029611121 ) ) ;
#12594 = AXIS2_PLACEMENT_3D ( 'NONE', #9214, #16067, #3973 ) ;
#12595 = ORIENTED_EDGE ( 'NONE', *, *, #16322, .T. ) ;
#12596 = CARTESIAN_POINT ( 'NONE',  ( -7.714727599197334307, -79.05312499999985221, -18.62500000000064659 ) ) ;
#12597 = ADVANCED_FACE ( 'NONE', ( #13429 ), #1318, .T. ) ;
#12598 = CARTESIAN_POINT ( 'NONE',  ( 11.62831264688102451, 48.17469404744644379, 6.858106635231019155 ) ) ;
#12599 = EDGE_CURVE ( 'NONE', #13643, #2583, #8830, .T. ) ;
#12600 = CARTESIAN_POINT ( 'NONE',  ( 13.50000000000000000, 65.43000000000000682, 1.653273178848926867E-15 ) ) ;
#12601 = CARTESIAN_POINT ( 'NONE',  ( -13.49999999999999822, 34.78000000000000114, -4.386415899144240349 ) ) ;
#12602=STYLED_ITEM('',(#17498),#3043);
#12603 = CARTESIAN_POINT ( 'NONE',  ( -0.6926531483078592899, 8.027905821154657673, 18.11545820097774850 ) ) ;
#12604 = CARTESIAN_POINT ( 'NONE',  ( -5.666818938165120834, 67.38588027987705686, -12.25310711623839133 ) ) ;
#12605 = CARTESIAN_POINT ( 'NONE',  ( 9.538709233711902776E-13, 3.087500000000011458, -11.37500000000000178 ) ) ;
#12606 = CARTESIAN_POINT ( 'NONE',  ( 8.670433428822322597, 54.01357483247397795, 10.35003895964909226 ) ) ;
#12607 = ORIENTED_EDGE ( 'NONE', *, *, #15617, .F. ) ;
#12608 = CARTESIAN_POINT ( 'NONE',  ( -3.191717032724610714, 64.29480952879987399, -13.11732287425230581 ) ) ;
#12609 = ORIENTED_EDGE ( 'NONE', *, *, #9500, .T. ) ;
#12610 = CARTESIAN_POINT ( 'NONE',  ( -9.604335505081937896, 34.55882025099123922, -9.493374980285292253 ) ) ;
#12611 = CARTESIAN_POINT ( 'NONE',  ( 9.538709233711902776E-13, -20.81249999999995026, -11.37500000000000000 ) ) ;
#12612 = CARTESIAN_POINT ( 'NONE',  ( 10.47449681190867210, 78.10467755407360357, 8.516757727679493684 ) ) ;
#12613 = CARTESIAN_POINT ( 'NONE',  ( -10.17530313047220680, 7.957378145380317847, -15.32050807568887940 ) ) ;
#12614 = AXIS2_PLACEMENT_3D ( 'NONE', #4782, #7445, #11325 ) ;
#12615 = EDGE_CURVE ( 'NONE', #10808, #7754, #14208, .T. ) ;
#12616 = CARTESIAN_POINT ( 'NONE',  ( 7.500000000000000888, -26.30006709664695563, -6.927727048493003359 ) ) ;
#12617 = CARTESIAN_POINT ( 'NONE',  ( 11.86550600985247250, 72.66835694352569419, -6.439119142892169023 ) ) ;
#12618 = CARTESIAN_POINT ( 'NONE',  ( 3.636496289402154414, 25.83000000000001961, 11.19198476289190758 ) ) ;
#12619 = CARTESIAN_POINT ( 'NONE',  ( -4.171729424061791036, 59.53000000000000114, 12.83926296998457239 ) ) ;
#12620 = CARTESIAN_POINT ( 'NONE',  ( -5.806291557865342234, 52.39132149430719210, -12.18757512875381721 ) ) ;
#12621 = CARTESIAN_POINT ( 'NONE',  ( -3.636496289402155746, 36.53000000000000114, 11.19198476289190936 ) ) ;
#12622 = CARTESIAN_POINT ( 'NONE',  ( -8.343458848123576743, 60.47999999999999687, -11.48378591275254301 ) ) ;
#12623 = CARTESIAN_POINT ( 'NONE',  ( 1.522075781121807969, 50.73472822943448080, 13.41392177511433559 ) ) ;
#12624 = CARTESIAN_POINT ( 'NONE',  ( 7.272992578804308828, -4.019999999999998685, 10.01041549318726709 ) ) ;
#12625 = CARTESIAN_POINT ( 'NONE',  ( 9.736523788050917005, 69.06556698226975755, 9.351906487042457528 ) ) ;
#12626 = CYLINDRICAL_SURFACE ( 'NONE', #16900, 5.000000000000000000 ) ;
#12627 = CARTESIAN_POINT ( 'NONE',  ( -7.999999999999776179, 0.000000000000000000, -17.32050807568887762 ) ) ;
#12628 = CARTESIAN_POINT ( 'NONE',  ( -18.62500000000000000, -98.82499999999978968, -1.562973063126292757E-12 ) ) ;
#12629 = CARTESIAN_POINT ( 'NONE',  ( -13.22250539961364169, 73.83308068845481387, -2.742208778312596795 ) ) ;
#12630 = CARTESIAN_POINT ( 'NONE',  ( -2.875760791593931984E-14, 76.17999999999999261, -13.50000000000000000 ) ) ;
#12631 = CARTESIAN_POINT ( 'NONE',  ( 8.000000000000023093, 0.000000000000000000, -17.32050807568876394 ) ) ;
#12632 = CARTESIAN_POINT ( 'NONE',  ( -7.416407864998737942, 1.246025403784429164, 10.20780970022447853 ) ) ;
#12633 = CARTESIAN_POINT ( 'NONE',  ( 15.00000000000000000, 0.000000000000000000, 1.256933281983527907E-12 ) ) ;
#12634 = CARTESIAN_POINT ( 'NONE',  ( -11.76794919243112325, -8.070000000000000284, -2.602085213965210642E-15 ) ) ;
#12635 = CARTESIAN_POINT ( 'NONE',  ( -11.76794919243112325, 41.78000000000000114, -3.823638476888998827 ) ) ;
#12636 = UNCERTAINTY_MEASURE_WITH_UNIT (LENGTH_MEASURE( 1.000000000000000082E-05 ), #9829, 'distance_accuracy_value', 'NONE');
#12637 = CARTESIAN_POINT ( 'NONE',  ( -10.92172942406178926, -13.36999999999999922, -7.935100905948389460 ) ) ;
#12638 = EDGE_CURVE ( 'NONE', #42, #8284, #12900, .T. ) ;
#12639 = CARTESIAN_POINT ( 'NONE',  ( -7.169881344235224496, 32.41318569726487908, 11.43868762491521451 ) ) ;
#12640 = FACE_OUTER_BOUND ( 'NONE', #757, .T. ) ;
#12641 = CARTESIAN_POINT ( 'NONE',  ( 11.76794919243112325, 31.27999999999998693, 3.823638476888996607 ) ) ;
#12642 = CARTESIAN_POINT ( 'NONE',  ( 1.963551943317787263, 52.10952655783576404, -13.36279640122861423 ) ) ;
#12643 = CARTESIAN_POINT ( 'NONE',  ( -4.076052042102673134, 38.53349475998775375, 12.87062638305022411 ) ) ;
#12644 = CARTESIAN_POINT ( 'NONE',  ( 0.2077865973656172205, 37.17252950262063393, -13.49854835976931078 ) ) ;
#12645 = CARTESIAN_POINT ( 'NONE',  ( -8.343458848123582072, 70.37999999999999545, 11.48378591275253768 ) ) ;
#12646 = CARTESIAN_POINT ( 'NONE',  ( 0.000000000000000000, 108.9300000000000068, -12.00000000000000178 ) ) ;
#12647 = CARTESIAN_POINT ( 'NONE',  ( 6.600044012045160891, 62.92306809907158538, 11.77869433798020715 ) ) ;
#12648 = CARTESIAN_POINT ( 'NONE',  ( 3.074525348032466798, 41.79056361433298861, 13.14524077292679749 ) ) ;
#12649 = CARTESIAN_POINT ( 'NONE',  ( 10.61485236059771786, 48.74751858167648066, -8.341608621204406049 ) ) ;
#12650 = CARTESIAN_POINT ( 'NONE',  ( 11.76794919243112325, 26.43000000000001037, 1.734723475976807094E-15 ) ) ;
#12651 = ORIENTED_EDGE ( 'NONE', *, *, #2014, .T. ) ;
#12652 = CARTESIAN_POINT ( 'NONE',  ( 11.76794919243112325, 67.43000000000000682, 1.441158131103945434E-15 ) ) ;
#12653 = CARTESIAN_POINT ( 'NONE',  ( 7.714727599200456254, -79.12187499999980389, -18.62499999999935341 ) ) ;
#12654 = CARTESIAN_POINT ( 'NONE',  ( -8.043339635996302306, -39.54374999999990337, -8.043339635997654113 ) ) ;
#12655 = EDGE_LOOP ( 'NONE', ( #6749, #2498 ) ) ;
#12656 = CARTESIAN_POINT ( 'NONE',  ( -0.5621853200489609348, 43.20021404884155203, -13.48847943194547483 ) ) ;
#12657 = CARTESIAN_POINT ( 'NONE',  ( -8.000000000000161648, 7.170682760640493925, 19.79706521687760201 ) ) ;
#12658 = VECTOR ( 'NONE', #16753, 1000.000000000000000 ) ;
#12659 = CARTESIAN_POINT ( 'NONE',  ( -4.171729424061787483, 5.330000000000001847, -12.83926296998457417 ) ) ;
#12660 = CARTESIAN_POINT ( 'NONE',  ( 7.714727599200458030, -3.121874999999992628, -18.62499999999935341 ) ) ;
#12661 = CARTESIAN_POINT ( 'NONE',  ( 8.311444000958445599, 65.99692735864155679, 10.63876800420476698 ) ) ;
#12662 = CARTESIAN_POINT ( 'NONE',  ( -13.49999999999999822, 82.78000000000001535, -4.386415899144240349 ) ) ;
#12663 = CARTESIAN_POINT ( 'NONE',  ( 11.76794919243112325, 61.27999999999999403, 3.823638476888996607 ) ) ;
#12664 = CARTESIAN_POINT ( 'NONE',  ( 6.750022565184456980, 31.92926174983937671, 11.69132992304556673 ) ) ;
#12665 = CARTESIAN_POINT ( 'NONE',  ( 11.76794919243112680, 61.57999999999999829, -3.823638476888993942 ) ) ;
#12666 = CARTESIAN_POINT ( 'NONE',  ( -12.53713441344856072, 46.74807280042572444, -5.007212535617639126 ) ) ;
#12667 = CARTESIAN_POINT ( 'NONE',  ( 6.273726922098238568, 45.95023082440073381, -11.95538543147346822 ) ) ;
#12668 = CARTESIAN_POINT ( 'NONE',  ( 8.093548673611641320, 69.87292072123501896, -10.80485039633414601 ) ) ;
#12669 = CARTESIAN_POINT ( 'NONE',  ( -7.779800476318354832E-16, 7.813974596215564006, 12.00000000000000355 ) ) ;
#12670 = CARTESIAN_POINT ( 'NONE',  ( 11.28924783770012219, 30.70771545723502172, -7.402899756116059216 ) ) ;
#12671 = AXIS2_PLACEMENT_3D ( 'NONE', #4160, #2639, #8070 ) ;
#12672 = EDGE_CURVE ( 'NONE', #16820, #7842, #10790, .T. ) ;
#12673 = CARTESIAN_POINT ( 'NONE',  ( -13.36489353327162632, 55.86322898162038086, -1.909449360262173379 ) ) ;
#12674 = CARTESIAN_POINT ( 'NONE',  ( 10.00000000000002132, 0.000000000000000000, -17.32050807568876394 ) ) ;
#12675 = CARTESIAN_POINT ( 'NONE',  ( 12.51119357652121344, 33.24557417593518238, 5.072678182924500234 ) ) ;
#12676 = PLANE ( 'NONE',  #360 ) ;
#12677 = CARTESIAN_POINT ( 'NONE',  ( 8.190820164315349317, 39.86853779885616689, -10.73135278157234396 ) ) ;
#12678 = ORIENTED_EDGE ( 'NONE', *, *, #17355, .T. ) ;
#12679 = CARTESIAN_POINT ( 'NONE',  ( -13.46074512384716115, 61.89434089339735579, -1.032255895472621088 ) ) ;
#12680 = EDGE_LOOP ( 'NONE', ( #10314, #15584, #3844, #10660 ) ) ;
#12681 = CARTESIAN_POINT ( 'NONE',  ( -13.21933525180101121, 40.83269136074343919, -2.754417799056112059 ) ) ;
#12682 = CARTESIAN_POINT ( 'NONE',  ( 11.76794919243112680, -18.42000000000000171, -3.823638476888993942 ) ) ;
#12683 = CARTESIAN_POINT ( 'NONE',  ( -18.62500000000064659, -9.365624999999976552, 7.714727599197335195 ) ) ;
#12684 = CARTESIAN_POINT ( 'NONE',  ( 13.01373734262449311, 48.30174901136457066, 3.592500545224007968 ) ) ;
#12685 = CARTESIAN_POINT ( 'NONE',  ( -8.000000000000143885, 7.773118517290097174, 17.32050807568870709 ) ) ;
#12686 = CARTESIAN_POINT ( 'NONE',  ( -10.92172942406179104, 35.22999999999999687, 7.935100905948387684 ) ) ;
#12687 =( BOUNDED_CURVE ( )  B_SPLINE_CURVE ( 2, ( #1616, #16551, #1526, #1347, #13460, #12321, #298, #16370, #1435, #15214, #4458, #6853, #10912 ),
 .UNSPECIFIED., .F., .T. ) 
 B_SPLINE_CURVE_WITH_KNOTS ( ( 3, 2, 2, 2, 2, 2, 3 ),
 ( 0.01714606201576732852, 0.02090154730321778717, 0.02841251787809168788, 0.03592348845296558513, 0.04343445902783955870, 0.05094542960271345594, 0.05470091489015040803 ),
 .UNSPECIFIED. ) 
 CURVE ( )  GEOMETRIC_REPRESENTATION_ITEM ( )  RATIONAL_B_SPLINE_CURVE ( ( 0.9755282581475768211, 0.9755282581474891135, 1.000000000000000000, 0.9510565162951536422, 1.000000000000000000, 0.9510565162951536422, 1.000000000000000000, 0.9510565162951536422, 1.000000000000000000, 0.9510565162951536422, 1.000000000000000000, 0.9755282581475768211, 0.9755282581475768211 ) ) 
 REPRESENTATION_ITEM ( '' )  );
#12688 = CARTESIAN_POINT ( 'NONE',  ( -0.03222258848736525572, 46.18115845073967307, -13.49996702218131261 ) ) ;
#12689 = EDGE_CURVE ( 'NONE', #15652, #4019, #786, .T. ) ;
#12690 = LINE ( 'NONE', #12948, #2019 ) ;
#12691 = CARTESIAN_POINT ( 'NONE',  ( -11.37499999999960743, -66.63437499999983515, -4.711679271994912099 ) ) ;
#12692 = CARTESIAN_POINT ( 'NONE',  ( 10.55718600268835772, 54.10925673300133099, 8.414815218569547284 ) ) ;
#12693 = AXIS2_PLACEMENT_3D ( 'NONE', #6105, #11571, #3691 ) ;
#12694 = ORIENTED_EDGE ( 'NONE', *, *, #13650, .F. ) ;
#12695 = CARTESIAN_POINT ( 'NONE',  ( -10.08098277730616310, 64.58357994695883519, -8.980069834276186214 ) ) ;
#12696 = ORIENTED_EDGE ( 'NONE', *, *, #14898, .F. ) ;
#12697 = FACE_OUTER_BOUND ( 'NONE', #5254, .T. ) ;
#12698 = CARTESIAN_POINT ( 'NONE',  ( -10.16207160523757835, 34.58782041647135941, -8.887247792507393385 ) ) ;
#12699 = CARTESIAN_POINT ( 'NONE',  ( 11.37499999999960210, -15.60937499999996270, 4.711679271994918317 ) ) ;
#12700 = CARTESIAN_POINT ( 'NONE',  ( 8.623259911401813582, 78.01131858175091338, 10.38704685952772699 ) ) ;
#12701 = LINE ( 'NONE', #4396, #12658 ) ;
#12702 = FACE_OUTER_BOUND ( 'NONE', #17011, .T. ) ;
#12703 = CARTESIAN_POINT ( 'NONE',  ( 7.500000000000003553, -27.55009420329275471, -3.560038493048078401 ) ) ;
#12704 = CARTESIAN_POINT ( 'NONE',  ( 11.31643680712456401, 72.15395803400841146, 7.362692955525563576 ) ) ;
#12705 = CARTESIAN_POINT ( 'NONE',  ( 11.76794919243112325, 29.43000000000001037, 1.734723475976807094E-15 ) ) ;
#12706 = CARTESIAN_POINT ( 'NONE',  ( -13.49999999999999822, 65.07999999999999829, 4.386415899144235908 ) ) ;
#12707 = CARTESIAN_POINT ( 'NONE',  ( -5.794542289981962746, 52.39086140184792129, -12.19316736257134437 ) ) ;
#12708 = CARTESIAN_POINT ( 'NONE',  ( 3.636496289402157078, 35.03000000000000114, -11.19198476289190936 ) ) ;
#12709 = CARTESIAN_POINT ( 'NONE',  ( 11.76794919243112325, -15.57000000000000028, 1.734723475976807094E-15 ) ) ;
#12710 = CARTESIAN_POINT ( 'NONE',  ( -8.691771469529815392E-16, 55.67999999999999972, 14.19474002721660355 ) ) ;
#12711 = CARTESIAN_POINT ( 'NONE',  ( -10.00000000000014211, 0.000000000000000000, 17.32050807568869288 ) ) ;
#12712 = CARTESIAN_POINT ( 'NONE',  ( 11.76794919243112325, -6.569999999999999396, 1.734723475976807094E-15 ) ) ;
#12713 = CARTESIAN_POINT ( 'NONE',  ( 9.990009898246189124, 69.07869612477813348, 9.080182975746776464 ) ) ;
#12714 = CARTESIAN_POINT ( 'NONE',  ( 9.708203932499390731, 2.863974596215587365, -7.053423027509691856 ) ) ;
#12715 = EDGE_CURVE ( 'NONE', #4556, #14181, #1367, .T. ) ;
#12716 = DIRECTION ( 'NONE',  ( 0.000000000000000000, 0.000000000000000000, -1.000000000000000000 ) ) ;
#12717 = CARTESIAN_POINT ( 'NONE',  ( 13.16986379959833897, -88.41874999999980389, 13.16986379960055409 ) ) ;
#12718 = CARTESIAN_POINT ( 'NONE',  ( -10.55719944458992998, 73.60929019257851280, -8.414036521270118030 ) ) ;
#12719 = CARTESIAN_POINT ( 'NONE',  ( 17.42428528562844292, 0.000000000000000000, 19.29752010712858024 ) ) ;
#12720 = CARTESIAN_POINT ( 'NONE',  ( -11.76794919243112325, 80.92999999999767624, -5.919446256302011733E-11 ) ) ;
#12721 = CARTESIAN_POINT ( 'NONE',  ( 8.671371105899947196, 8.051439890486543405, -15.81984194950172906 ) ) ;
#12722 = CARTESIAN_POINT ( 'NONE',  ( -8.343458848123576743, 26.48000000000001464, -11.48378591275254301 ) ) ;
#12723 = CARTESIAN_POINT ( 'NONE',  ( -7.272992578804307939, -11.51999999999999957, -10.01041549318726886 ) ) ;
#12724 = CARTESIAN_POINT ( 'NONE',  ( -7.272992578804310604, 42.37999999999999545, 10.01041549318726886 ) ) ;
#12725 = DIRECTION ( 'NONE',  ( 1.000000000000000000, 0.000000000000000000, 0.000000000000000000 ) ) ;
#12726 = CARTESIAN_POINT ( 'NONE',  ( -11.26568359562893029, 32.20920359819594125, 7.438710005716663964 ) ) ;
#12727 = CARTESIAN_POINT ( 'NONE',  ( 5.795435194651767041, 74.89090867474413926, 12.19293766284020997 ) ) ;
#12728 = CYLINDRICAL_SURFACE ( 'NONE', #8270, 13.50000000000000000 ) ;
#12729 = CARTESIAN_POINT ( 'NONE',  ( -4.171729424061791036, 79.53000000000000114, 12.83926296998457239 ) ) ;
#12730 = CARTESIAN_POINT ( 'NONE',  ( 2.775048885307294100, 52.08055395342481120, -13.21813026032616456 ) ) ;
#12731 = DIRECTION ( 'NONE',  ( 0.000000000000000000, 0.000000000000000000, 1.000000000000000000 ) ) ;
#12732 = EDGE_CURVE ( 'NONE', #15368, #16820, #4774, .T. ) ;
#12733 = CARTESIAN_POINT ( 'NONE',  ( 15.00000000000000000, -99.89999999999999147, 0.000000000000000000 ) ) ;
#12734 = CARTESIAN_POINT ( 'NONE',  ( 0.000000000000000000, 80.93000000000000682, 0.000000000000000000 ) ) ;
#12735 = CARTESIAN_POINT ( 'NONE',  ( -0.2547729068321639145, 49.18915660688823976, -13.49793348477203203 ) ) ;
#12736 = CARTESIAN_POINT ( 'NONE',  ( 2.567202442714003219, 62.77235785574046645, 13.25368192155630709 ) ) ;
#12737 = CARTESIAN_POINT ( 'NONE',  ( 3.053862296787171360, 41.78983512861384497, 13.15006426398930550 ) ) ;
#12738 = CARTESIAN_POINT ( 'NONE',  ( 10.67465755508037617, 48.74414866033003335, -8.264490526360749101 ) ) ;
#12739 = CARTESIAN_POINT ( 'NONE',  ( 3.636496289402157078, 18.03000000000001890, -11.19198476289190936 ) ) ;
#12740 = ORIENTED_EDGE ( 'NONE', *, *, #15825, .F. ) ;
#12741 = CARTESIAN_POINT ( 'NONE',  ( 9.520470885617715595, 64.12999999999999545, 6.917026985038134512 ) ) ;
#12742 = CARTESIAN_POINT ( 'NONE',  ( -7.714727599197334307, -81.20312499999978684, -18.62500000000064659 ) ) ;
#12743 = CARTESIAN_POINT ( 'NONE',  ( 4.711679271994910323, -53.07187499999987068, -11.37499999999960387 ) ) ;
#12744 = CARTESIAN_POINT ( 'NONE',  ( 13.49999999999999822, 3.280000000000003801, 4.386415899144237684 ) ) ;
#12745 = CARTESIAN_POINT ( 'NONE',  ( 9.520470885617717371, 32.73000000000001108, -6.917026985038131848 ) ) ;
#12746 = CARTESIAN_POINT ( 'NONE',  ( -0.7362654489741128350, 80.93000000000000682, -13.00758670407025086 ) ) ;
#12747 = CARTESIAN_POINT ( 'NONE',  ( -7.714727599197334307, -71.80312499999982379, -18.62500000000064304 ) ) ;
#12748 = CARTESIAN_POINT ( 'NONE',  ( 5.706916115397674183, 65.88744019540719421, 12.23443642958042687 ) ) ;
#12749 = DIRECTION ( 'NONE',  ( 1.000000000000000000, 0.000000000000000000, 0.000000000000000000 ) ) ;
#12750 = CARTESIAN_POINT ( 'NONE',  ( -11.76794919243112325, 50.77999999999998693, -3.823638476888998827 ) ) ;
#12751 = CARTESIAN_POINT ( 'NONE',  ( -9.520470885617717371, 57.23000000000000398, 6.917026985038133624 ) ) ;
#12752 = CARTESIAN_POINT ( 'NONE',  ( -12.97183641456126502, 46.79586893643946865, -3.748799059863759275 ) ) ;
#12753 = CARTESIAN_POINT ( 'NONE',  ( 12.62323547485571851, 45.60479695812286138, -4.831092889884269326 ) ) ;
#12754 = CARTESIAN_POINT ( 'NONE',  ( 5.666431094655353107, 69.97415835491503344, -12.25323033163396680 ) ) ;
#12755 = AXIS2_PLACEMENT_3D ( 'NONE', #6935, #13709, #5784 ) ;
#12756 = CARTESIAN_POINT ( 'NONE',  ( 0.1775006636059767717, 8.062177826491092603, 18.00000000000001421 ) ) ;
#12757 = CARTESIAN_POINT ( 'NONE',  ( 5.837233680499599231, 30.96745156617631523, -12.17279074635751535 ) ) ;
#12758 = CARTESIAN_POINT ( 'NONE',  ( -12.15097179258997073, 55.71389053688777437, -5.882769356534193861 ) ) ;
#12759 = CARTESIAN_POINT ( 'NONE',  ( -2.759338081070636051, 50.58068028277337191, 13.21652401455469850 ) ) ;
#12760 = CARTESIAN_POINT ( 'NONE',  ( 13.29140006584865574, 33.34684006576951276, 2.364050045256024468 ) ) ;
#12761 = CARTESIAN_POINT ( 'NONE',  ( 4.264411549263888546, 43.02666127736967638, -12.80881877248479128 ) ) ;
#12762 = CARTESIAN_POINT ( 'NONE',  ( 11.16754829665910798, 39.71527879939828409, -7.585325781705508419 ) ) ;
#12763 = ORIENTED_EDGE ( 'NONE', *, *, #7336, .F. ) ;
#12764 = CARTESIAN_POINT ( 'NONE',  ( -13.45264947251579102, 61.96924832227834656, 1.132187044750279536 ) ) ;
#12765 = VERTEX_POINT ( 'NONE', #12816 ) ;
#12766 = ORIENTED_EDGE ( 'NONE', *, *, #10937, .T. ) ;
#12767 = CARTESIAN_POINT ( 'NONE',  ( 2.279995255611139653E-15, -17.82000000000000028, -12.37355403259654985 ) ) ;
#12768 = CARTESIAN_POINT ( 'NONE',  ( 13.16986379960055054, -35.38124999999991616, -13.16986379959834430 ) ) ;
#12769 = CIRCLE ( 'NONE', #6287, 9.000000000000001776 ) ;
#12770 = CARTESIAN_POINT ( 'NONE',  ( 8.312300566215480302, 57.86311205854902795, -10.64140145696314121 ) ) ;
#12771 = CARTESIAN_POINT ( 'NONE',  ( 5.638949650228808785, 78.97550847713628741, -12.27579838479350194 ) ) ;
#12772 = ADVANCED_FACE ( 'NONE', ( #1841 ), #12728, .T. ) ;
#12773 = CARTESIAN_POINT ( 'NONE',  ( 3.636496289402154414, 75.83000000000001251, 11.19198476289190936 ) ) ;
#12774 = CARTESIAN_POINT ( 'NONE',  ( 13.50000000000000355, 41.57999999999999119, -4.386415899144233244 ) ) ;
#12775 = CARTESIAN_POINT ( 'NONE',  ( 9.854515491449854281, 2.875466159201984032E-15, -7.259896930270302029 ) ) ;
#12776 = CARTESIAN_POINT ( 'NONE',  ( -4.302195761316967015, 46.33469344025497350, -12.79681310502842884 ) ) ;
#12777 = LINE ( 'NONE', #4999, #4867 ) ;
#12778 = CARTESIAN_POINT ( 'NONE',  ( 4.711679271994911211, -29.17187499999991118, -11.37499999999960743 ) ) ;
#12779 = VECTOR ( 'NONE', #4373, 999.9999999999998863 ) ;
#12780 = CARTESIAN_POINT ( 'NONE',  ( 3.313926305061611455, 53.79912973232266893, 13.08694846433931858 ) ) ;
#12781 = ORIENTED_EDGE ( 'NONE', *, *, #1130, .T. ) ;
#12782 = FACE_OUTER_BOUND ( 'NONE', #6448, .T. ) ;
#12783 = EDGE_LOOP ( 'NONE', ( #15626, #5256, #12694, #8342 ) ) ;
#12784 = B_SPLINE_CURVE_WITH_KNOTS ( 'NONE', 3,
 ( #4848, #694, #16686, #4593, #2085, #7510, #15437, #8761, #15261, #12721, #15520, #8927, #14117, #2171, #12892, #7248, #15348, #7429 ),
 .UNSPECIFIED., .F., .F.,
 ( 4, 2, 2, 2, 2, 2, 2, 2, 4 ),
 ( 2.030049010680397696E-07, 0.0003947283216049050393, 0.0007892536383087419768, 0.001183778955012579131, 0.001578304271716416069, 0.001972829588420253223, 0.002367354905124090161, 0.002761880221827927098, 0.003156405538531764036 ),
 .UNSPECIFIED. ) ;
#12785 = CARTESIAN_POINT ( 'NONE',  ( 2.000359907488380884, 67.10810958415484606, -13.35850880710533772 ) ) ;
#12786 = CARTESIAN_POINT ( 'NONE',  ( -8.288051004685030421, 34.49586041775943102, -10.65699721998313976 ) ) ;
#12787 = CARTESIAN_POINT ( 'NONE',  ( -13.49999999999999822, 17.78000000000001535, -4.386415899144240349 ) ) ;
#12788 = CARTESIAN_POINT ( 'NONE',  ( -9.552639591052204498E-13, -36.38749999999993179, 11.37499999999999645 ) ) ;
#12789 = CARTESIAN_POINT ( 'NONE',  ( 5.969853497853632618, 77.89748442894395453, 12.11621569323665781 ) ) ;
#12790 = CARTESIAN_POINT ( 'NONE',  ( -15.49921147158550916, 8.062143943920768052, 9.154805866618353605 ) ) ;
#12791 = CARTESIAN_POINT ( 'NONE',  ( 15.67790026899618461, 8.062143948122718839, 8.845307762532291562 ) ) ;
#12792 = DIRECTION ( 'NONE',  ( 0.000000000000000000, 0.000000000000000000, 1.000000000000000000 ) ) ;
#12793 = CARTESIAN_POINT ( 'NONE',  ( 12.17897594257505034, 72.64436298052412155, -5.840729639915025473 ) ) ;
#12794 = CARTESIAN_POINT ( 'NONE',  ( 11.76794919243112325, 26.43000000000001037, 1.734723475976807094E-15 ) ) ;
#12795 = CARTESIAN_POINT ( 'NONE',  ( 4.171729424061789260, 62.82999999999999829, 12.83926296998457417 ) ) ;
#12796 = CARTESIAN_POINT ( 'NONE',  ( -0.5918238176221393143, 52.20127980115676536, -13.49999999999999822 ) ) ;
#12797 = AXIS2_PLACEMENT_3D ( 'NONE', #8673, #6187, #435 ) ;
#12798 = CARTESIAN_POINT ( 'NONE',  ( 11.76794919243112325, 34.28000000000000114, 3.823638476888996607 ) ) ;
#12799 = CARTESIAN_POINT ( 'NONE',  ( -3.636496289402156190, -16.46999999999999886, 11.19198476289190758 ) ) ;
#12800 = CARTESIAN_POINT ( 'NONE',  ( -13.49999999999999822, 60.78000000000000114, -4.386415899144240349 ) ) ;
#12801 = DIRECTION ( 'NONE',  ( 0.000000000000000000, 1.000000000000000000, 0.000000000000000000 ) ) ;
#12802 = CARTESIAN_POINT ( 'NONE',  ( 3.479075845151533564, 68.80513213033660236, 13.04407958699342096 ) ) ;
#12803 = CARTESIAN_POINT ( 'NONE',  ( -7.714727599197335195, -38.50312499999991189, -18.62500000000064304 ) ) ;
#12804 = CARTESIAN_POINT ( 'NONE',  ( 2.138189944381231555, 72.10311857767972299, -13.50000000000000178 ) ) ;
#12805 = CARTESIAN_POINT ( 'NONE',  ( -13.16986379959834252, -39.54374999999990337, -13.16986379960055054 ) ) ;
#12806 = CARTESIAN_POINT ( 'NONE',  ( -13.46101605912647337, 73.89364307768008189, -1.052211620652566681 ) ) ;
#12807 = CARTESIAN_POINT ( 'NONE',  ( -9.269880003010733560, 76.54218929687127115, -9.814641767077731060 ) ) ;
#12808 = CARTESIAN_POINT ( 'NONE',  ( 1.900613283894434735, 7.622906826104705047, 12.00000000000000000 ) ) ;
#12809 = CARTESIAN_POINT ( 'NONE',  ( -7.499999999999999112, 102.9299999999999073, -9.367496997597655195 ) ) ;
#12810 = ORIENTED_EDGE ( 'NONE', *, *, #744, .F. ) ;
#12811 = CARTESIAN_POINT ( 'NONE',  ( 3.636496289402154414, 33.82999999999999829, 11.19198476289190936 ) ) ;
#12812 = CARTESIAN_POINT ( 'NONE',  ( 3.708203932499368527, 4.963974596215562585, 11.41267819554184193 ) ) ;
#12813 = CARTESIAN_POINT ( 'NONE',  ( -9.816093411897769627, 32.29071182833408926, 9.278652180130679383 ) ) ;
#12814 = CARTESIAN_POINT ( 'NONE',  ( 1.061297819423365540, 74.71813576689515912, 13.45990699938060331 ) ) ;
#12815 = EDGE_CURVE ( 'NONE', #17188, #6168, #1268, .T. ) ;
#12816 = CARTESIAN_POINT ( 'NONE',  ( -10.99999999999979394, 7.773118517290098950, -15.58845726812003996 ) ) ;
#12817 = CARTESIAN_POINT ( 'NONE',  ( 0.1963306558083189324, 30.65984393938648722, 13.47512034797125580 ) ) ;
#12818 = CARTESIAN_POINT ( 'NONE',  ( 12.61419996821527789, 51.60431945238178741, -4.809772638418851720 ) ) ;
#12819 = B_SPLINE_CURVE_WITH_KNOTS ( 'NONE', 3,
 ( #8766, #3519, #14121, #1839 ),
 .UNSPECIFIED., .F., .F.,
 ( 4, 4 ),
 ( 0.008786844460939023313, 0.01643317035798799036 ),
 .UNSPECIFIED. ) ;
#12820 = CARTESIAN_POINT ( 'NONE',  ( -12.47471083728540719, 38.11787751918529921, 5.160988080696901292 ) ) ;
#12821 = CARTESIAN_POINT ( 'NONE',  ( 11.96006256146126390, 36.66123345659914889, -6.261549132648513094 ) ) ;
#12822 = CARTESIAN_POINT ( 'NONE',  ( 9.538709233711902776E-13, -11.41249999999998899, -11.37499999999999645 ) ) ;
#12823 = PLANE ( 'NONE',  #5456 ) ;
#12824 = CARTESIAN_POINT ( 'NONE',  ( -24.73863375370603634, 0.000000000000000000, 7.999999999999761080 ) ) ;
#12825 = CARTESIAN_POINT ( 'NONE',  ( -2.138189944381257757, 60.25688142232026934, -13.49999999999999289 ) ) ;
#12826 = CARTESIAN_POINT ( 'NONE',  ( -11.76349012782661951, 80.93000000000003524, 2.235278043115120461 ) ) ;
#12827 = CARTESIAN_POINT ( 'NONE',  ( 12.26213682806825567, 48.63686586570011627, -5.647125736108378646 ) ) ;
#12828 = CARTESIAN_POINT ( 'NONE',  ( -7.409984580736203970E-16, 7.679999999999995275, 12.37355403259654985 ) ) ;
#12829 = LINE ( 'NONE', #13083, #8379 ) ;
#12830 = ORIENTED_EDGE ( 'NONE', *, *, #13515, .T. ) ;
#12831 = CARTESIAN_POINT ( 'NONE',  ( -11.76794919243112325, 62.92999999999999972, -2.882316262207890869E-15 ) ) ;
#12832 = CARTESIAN_POINT ( 'NONE',  ( -9.552639591052204498E-13, -21.88749999999992824, 11.37500000000000178 ) ) ;
#12833 = CARTESIAN_POINT ( 'NONE',  ( -11.37499999999960387, -40.58437499999990905, -4.711679271994911211 ) ) ;
#12834 = CARTESIAN_POINT ( 'NONE',  ( -13.49999999999999822, -0.9200000000000014833, 4.386415899144235908 ) ) ;
#12835 = CARTESIAN_POINT ( 'NONE',  ( -11.76794919243112325, 33.93000000000001393, -2.602085213965210642E-15 ) ) ;
#12836 = CARTESIAN_POINT ( 'NONE',  ( 0.9520164539180778762, 76.14576922985241936, -13.46646205020914699 ) ) ;
#12837 = EDGE_CURVE ( 'NONE', #9800, #6684, #16868, .T. ) ;
#12838 = CARTESIAN_POINT ( 'NONE',  ( 18.62500000000064304, -34.34062499999991758, -7.714727599197334307 ) ) ;
#12839 = AXIS2_PLACEMENT_3D ( 'NONE', #7601, #7432, #15787 ) ;
#12840 = CARTESIAN_POINT ( 'NONE',  ( 11.86519348393725970, 66.19162581074351692, 6.439609381232799024 ) ) ;
#12841 = CARTESIAN_POINT ( 'NONE',  ( -13.49999999999999822, 80.07999999999998408, 4.386415899144235908 ) ) ;
#12842 = CARTESIAN_POINT ( 'NONE',  ( 11.76794919243112325, 49.42999999999999972, 1.441158131103945434E-15 ) ) ;
#12843 = CARTESIAN_POINT ( 'NONE',  ( -9.954157355241310512, 59.28317716132346504, 9.119471290265320107 ) ) ;
#12844 = CARTESIAN_POINT ( 'NONE',  ( 10.52479684053763620, 45.75252738753766124, -8.454649685126563341 ) ) ;
#12845 = CARTESIAN_POINT ( 'NONE',  ( 8.136481847135470957, 69.87099141200431518, -10.77264556894015257 ) ) ;
#12846 = CARTESIAN_POINT ( 'NONE',  ( 13.04595580355921136, 30.55377996617673375, -3.472152230004342144 ) ) ;
#12847 = CARTESIAN_POINT ( 'NONE',  ( -13.30909409913599006, 55.85048046686320333, -2.263500039713061796 ) ) ;
#12848 = CARTESIAN_POINT ( 'NONE',  ( -3.859537734194087744, 50.54122529663226260, 12.93654704252784882 ) ) ;
#12849 = CARTESIAN_POINT ( 'NONE',  ( 9.846585001760786326, 63.78875900491937045, -9.235520396473821947 ) ) ;
#12850 = CARTESIAN_POINT ( 'NONE',  ( 3.028015045671256900, 43.07112457749870060, -13.15637380351495089 ) ) ;
#12851 = CARTESIAN_POINT ( 'NONE',  ( 12.04987116223745147, 39.65426265503597136, -6.087320985860698030 ) ) ;
#12852 = ORIENTED_EDGE ( 'NONE', *, *, #15881, .F. ) ;
#12853 = CARTESIAN_POINT ( 'NONE',  ( -13.20951207043308351, 61.83148949826453844, -2.786434271337515867 ) ) ;
#12854 = ORIENTED_EDGE ( 'NONE', *, *, #12423, .F. ) ;
#12855 = ORIENTED_EDGE ( 'NONE', *, *, #11299, .T. ) ;
#12856 = CARTESIAN_POINT ( 'NONE',  ( -13.50000000000000000, 34.93000000000001393, -3.469446951953614189E-15 ) ) ;
#12857 = CARTESIAN_POINT ( 'NONE',  ( -18.62500000000000000, -24.97499999999994102, -1.562973063126292555E-12 ) ) ;
#12858 = CARTESIAN_POINT ( 'NONE',  ( 13.08213917803373327, 48.31138509259425717, 3.332853635039773721 ) ) ;
#12859 = EDGE_CURVE ( 'NONE', #149, #225, #4175, .T. ) ;
#12860 = CARTESIAN_POINT ( 'NONE',  ( 10.49489484557887664, 57.75417860629620037, -8.491615491609847410 ) ) ;
#12861 = CARTESIAN_POINT ( 'NONE',  ( 4.440276171078080480, 79.02008338065117243, -12.75216793947442895 ) ) ;
#12862 = CARTESIAN_POINT ( 'NONE',  ( 2.272985001014427788E-15, 80.18000000000000682, -12.37355403259654985 ) ) ;
#12863 = CARTESIAN_POINT ( 'NONE',  ( 9.103919235555860467, 2.197554810170567017E-15, 9.934002182353431465 ) ) ;
#12864 = CARTESIAN_POINT ( 'NONE',  ( -1.645540471734166399, 7.815206720109966199, 18.85015970295419407 ) ) ;
#12865 = CARTESIAN_POINT ( 'NONE',  ( -5.441113646577659502, 0.000000000000000000, 25.42428528562849976 ) ) ;
#12866 = CARTESIAN_POINT ( 'NONE',  ( 9.538709233711902776E-13, -46.86249999999987637, -11.37500000000000178 ) ) ;
#12867 = VECTOR ( 'NONE', #16511, 1000.000000000000000 ) ;
#12868 = CARTESIAN_POINT ( 'NONE',  ( 11.54936908542054219, 54.16929694213506252, 6.991207511958483778 ) ) ;
#12869 = ORIENTED_EDGE ( 'NONE', *, *, #14875, .T. ) ;
#12870 = LINE ( 'NONE', #15670, #4720 ) ;
#12871 = EDGE_LOOP ( 'NONE', ( #12067, #14615, #9608, #13364 ) ) ;
#12872 = CARTESIAN_POINT ( 'NONE',  ( 5.334058230349888241, 66.98693642648522939, -12.40152507886732458 ) ) ;
#12873 = CARTESIAN_POINT ( 'NONE',  ( 11.37500000000039613, -24.94062499999995808, -4.711679271993002516 ) ) ;
#12874 = CYLINDRICAL_SURFACE ( 'NONE', #15920, 13.50000000000000000 ) ;
#12875 = CARTESIAN_POINT ( 'NONE',  ( -0.3076292557609190959, 59.66893862671528126, 13.49651329554702883 ) ) ;
#12876 = DIRECTION ( 'NONE',  ( 0.000000000000000000, 1.000000000000000000, 0.000000000000000000 ) ) ;
#12877 = CYLINDRICAL_SURFACE ( 'NONE', #11106, 8.999999999999998224 ) ;
#12878 = CARTESIAN_POINT ( 'NONE',  ( 11.48707053576665160, 72.16510984276516183, 7.092083023523681362 ) ) ;
#12879 = CARTESIAN_POINT ( 'NONE',  ( -7.272992578804307939, 30.48000000000000398, -10.01041549318726886 ) ) ;
#12880 =( GEOMETRIC_REPRESENTATION_CONTEXT ( 3 ) GLOBAL_UNCERTAINTY_ASSIGNED_CONTEXT ( ( #12636 ) ) GLOBAL_UNIT_ASSIGNED_CONTEXT ( ( #9829, #5754, #16424 ) ) REPRESENTATION_CONTEXT ( 'NONE', 'WORKASPACE' ) );
#12881 = CARTESIAN_POINT ( 'NONE',  ( 2.607531440858944223E-15, 49.17999999999999972, -14.19474002721660355 ) ) ;
#12882 = CARTESIAN_POINT ( 'NONE',  ( -11.20412284216293664, 52.64695269834547275, -7.531112085699138703 ) ) ;
#12883 = CARTESIAN_POINT ( 'NONE',  ( -13.49999999999999822, 52.07999999999999119, 4.386415899144235908 ) ) ;
#12884 = CARTESIAN_POINT ( 'NONE',  ( 8.343458848123583849, 77.88000000000000966, -11.48378591275253768 ) ) ;
#12885 = CARTESIAN_POINT ( 'NONE',  ( 1.801739650404782012, 68.74478696605716266, 13.37942991408443660 ) ) ;
#12886 = CARTESIAN_POINT ( 'NONE',  ( 18.62500000000000000, -49.94999999999988205, 1.560692158462880521E-12 ) ) ;
#12887 = DIRECTION ( 'NONE',  ( -0.000000000000000000, 1.000000000000000000, -0.000000000000000000 ) ) ;
#12888 = CARTESIAN_POINT ( 'NONE',  ( 7.714727599200458030, -19.77187499999995168, -18.62499999999934985 ) ) ;
#12889 = VECTOR ( 'NONE', #3778, 1000.000000000000227 ) ;
#12890 = CARTESIAN_POINT ( 'NONE',  ( -2.506966426393243630, 65.58985874448374886, 13.26518509152382030 ) ) ;
#12891 = CARTESIAN_POINT ( 'NONE',  ( -11.64508433789041675, 80.92999999999999261, -2.787474072191427510 ) ) ;
#12892 = CARTESIAN_POINT ( 'NONE',  ( 9.480101247244204998, 8.043253892159592411, -15.38474694851398183 ) ) ;
#12893 = CARTESIAN_POINT ( 'NONE',  ( -13.49999999999999822, 26.78000000000000114, -4.386415899144240349 ) ) ;
#12894 = VERTEX_POINT ( 'NONE', #2162 ) ;
#12895 = CARTESIAN_POINT ( 'NONE',  ( 4.171729424061791924, 51.03000000000000114, -12.83926296998457239 ) ) ;
#12896 = CARTESIAN_POINT ( 'NONE',  ( -4.345187459725349477, 40.33626392346928213, -12.78162779989500031 ) ) ;
#12897 = CARTESIAN_POINT ( 'NONE',  ( -12.71943797413999988, 31.76515268481853838, -4.567396653572560083 ) ) ;
#12898 = CARTESIAN_POINT ( 'NONE',  ( 3.539998177671969781, 74.80728451192426576, 13.02775590127090943 ) ) ;
#12899 = CARTESIAN_POINT ( 'NONE',  ( 12.05005302082176044, 60.20532830390902035, 6.102261332639054459 ) ) ;
#12900 = LINE ( 'NONE', #2093, #8552 ) ;
#12901 = DIRECTION ( 'NONE',  ( 1.000000000000000000, 0.000000000000000000, 0.000000000000000000 ) ) ;
#12902 = CARTESIAN_POINT ( 'NONE',  ( 4.171729424061791924, 72.03000000000000114, -12.83926296998457239 ) ) ;
#12903 = CARTESIAN_POINT ( 'NONE',  ( 13.49014888215909203, 51.44774366630825568, -0.5156731279918199684 ) ) ;
#12904 = CARTESIAN_POINT ( 'NONE',  ( -8.992785922287852785, 38.33140772955672304, 10.07305468610416987 ) ) ;
#12905 = CARTESIAN_POINT ( 'NONE',  ( 12.05351726939188062, 36.65397582186106717, -6.080038080744102125 ) ) ;
#12906 = CARTESIAN_POINT ( 'NONE',  ( 11.37500000000039613, -24.94062499999995808, -4.711679271993002516 ) ) ;
#12907 = EDGE_CURVE ( 'NONE', #12392, #11794, #6509, .T. ) ;
#12908 = DIRECTION ( 'NONE',  ( 0.000000000000000000, -1.000000000000000000, 0.000000000000000000 ) ) ;
#12909 = CARTESIAN_POINT ( 'NONE',  ( -4.484750243281778737, 77.51863919606381614, 12.74519890846088899 ) ) ;
#12910 = CYLINDRICAL_SURFACE ( 'NONE', #11100, 13.50000000000000000 ) ;
#12911 = CARTESIAN_POINT ( 'NONE',  ( 13.17195031443938547, 48.53499887136660362, -2.961669012155129010 ) ) ;
#12912 = CARTESIAN_POINT ( 'NONE',  ( -7.409984580736203970E-16, 16.68000000000000327, 12.37355403259654985 ) ) ;
#12913 = ORIENTED_EDGE ( 'NONE', *, *, #11125, .F. ) ;
#12914 = CARTESIAN_POINT ( 'NONE',  ( 3.636496289402157078, 62.03000000000000114, -11.19198476289190936 ) ) ;
#12915 = CARTESIAN_POINT ( 'NONE',  ( -4.711679271993003404, -14.60312499999994706, -11.37500000000039613 ) ) ;
#12916 = DIRECTION ( 'NONE',  ( 1.000000000000000000, 0.000000000000000000, 0.000000000000000000 ) ) ;
#12917 = CARTESIAN_POINT ( 'NONE',  ( -10.92172942406178926, -1.369999999999996110, -7.935100905948389460 ) ) ;
#12918 = CARTESIAN_POINT ( 'NONE',  ( 2.279995255611139653E-15, 33.17999999999999972, -12.37355403259654985 ) ) ;
#12919 = CARTESIAN_POINT ( 'NONE',  ( 1.293831188543124400, 76.13348380643110147, -13.43844946783898031 ) ) ;
#12920 = CARTESIAN_POINT ( 'NONE',  ( 1.561832610794586538E-12, -54.11249999999986926, -18.62500000000000000 ) ) ;
#12921 = CARTESIAN_POINT ( 'NONE',  ( 4.171729424061789260, 77.82999999999999829, 12.83926296998457417 ) ) ;
#12922 = CARTESIAN_POINT ( 'NONE',  ( 7.272992578804308828, 51.97999999999998977, 10.01041549318726709 ) ) ;
#12923 = CARTESIAN_POINT ( 'NONE',  ( -13.50510647780722095, 58.92757876024586494, -0.06544038226817162907 ) ) ;
#12924 = CARTESIAN_POINT ( 'NONE',  ( 11.88858366554402757, 45.19312755830633677, 6.405256951248860631 ) ) ;
#12925 = CARTESIAN_POINT ( 'NONE',  ( 5.622204590887941222, 69.97583870266406336, -12.27358394821601273 ) ) ;
#12926 = CARTESIAN_POINT ( 'NONE',  ( 1.753268986668952691E-06, 80.68004880551006863, 13.49999999999977263 ) ) ;
#12927 = CARTESIAN_POINT ( 'NONE',  ( 13.48213564506632522, 30.40254256736282557, 0.7883542253392303856 ) ) ;
#12928 = CARTESIAN_POINT ( 'NONE',  ( -13.47515042673155428, 55.90172887063787499, -0.8194478264856674965 ) ) ;
#12929 = EDGE_CURVE ( 'NONE', #14960, #8561, #4898, .T. ) ;
#12930 = CARTESIAN_POINT ( 'NONE',  ( -11.08263705370628749, 50.22048702777903628, 7.709197264984768871 ) ) ;
#12931 = CARTESIAN_POINT ( 'NONE',  ( 8.560836630084285304, 63.85167834306816559, -10.44139667627318069 ) ) ;
#12932 = CARTESIAN_POINT ( 'NONE',  ( 0.000000000000000000, 0.000000000000000000, 0.000000000000000000 ) ) ;
#12933 = CARTESIAN_POINT ( 'NONE',  ( 12.66463686987026271, 39.60059382856163523, -4.718913685864155383 ) ) ;
#12934 = ORIENTED_EDGE ( 'NONE', *, *, #14092, .F. ) ;
#12935 = CARTESIAN_POINT ( 'NONE',  ( -7.353569438412593584, 61.45463544861350869, -11.32146132068871580 ) ) ;
#12936 = VERTEX_POINT ( 'NONE', #12127 ) ;
#12937 = ORIENTED_EDGE ( 'NONE', *, *, #16787, .F. ) ;
#12938 = CARTESIAN_POINT ( 'NONE',  ( -8.343458848123576743, 28.48000000000001108, -11.48378591275254301 ) ) ;
#12939 = CARTESIAN_POINT ( 'NONE',  ( 7.714727599200458030, -19.77187499999995168, -18.62499999999934985 ) ) ;
#12940 = CARTESIAN_POINT ( 'NONE',  ( 9.541952228206893594, 48.05573085917402665, 9.550091761750962860 ) ) ;
#12941 = CARTESIAN_POINT ( 'NONE',  ( 10.04127278578228477, 57.77887113727757651, -9.033026199713900084 ) ) ;
#12942 = CARTESIAN_POINT ( 'NONE',  ( 11.13970935207611568, 78.71701762036461503, -7.626765219171713461 ) ) ;
#12943 = CARTESIAN_POINT ( 'NONE',  ( 11.76794919243112325, 76.42999999999999261, 1.441158131103945434E-15 ) ) ;
#12944 = CARTESIAN_POINT ( 'NONE',  ( 2.272985001014427788E-15, 83.17999999999999261, -12.37355403259654985 ) ) ;
#12945 = FACE_OUTER_BOUND ( 'NONE', #10725, .T. ) ;
#12946 = AXIS2_PLACEMENT_3D ( 'NONE', #6348, #17110, #5268 ) ;
#12947 = CARTESIAN_POINT ( 'NONE',  ( 7.499999999999996447, -8.000000000000000000, 9.367496997597600128 ) ) ;
#12948 = CARTESIAN_POINT ( 'NONE',  ( 0.000000000000000000, 30.93000000000001393, -13.50000000000000000 ) ) ;
#12949 = CARTESIAN_POINT ( 'NONE',  ( -4.711679271994916540, -37.49687499999989626, 11.37499999999960565 ) ) ;
#12950 = ADVANCED_FACE ( 'NONE', ( #4349 ), #1420, .T. ) ;
#12951 = CARTESIAN_POINT ( 'NONE',  ( -10.92172942406178926, 78.63000000000000966, -7.935100905948389460 ) ) ;
#12952 = CARTESIAN_POINT ( 'NONE',  ( 8.246725363360754457, 33.86600348702350516, -10.68840209571144939 ) ) ;
#12953 = ORIENTED_EDGE ( 'NONE', *, *, #5661, .T. ) ;
#12954 = CARTESIAN_POINT ( 'NONE',  ( -1.732050807569007977, 0.000000000000000000, 18.99999999999998224 ) ) ;
#12955 = ORIENTED_EDGE ( 'NONE', *, *, #15929, .F. ) ;
#12956 = LINE ( 'NONE', #15324, #14532 ) ;
#12957 = CARTESIAN_POINT ( 'NONE',  ( 11.37500000000039613, -41.59062499999991758, -4.711679271993002516 ) ) ;
#12958 = CIRCLE ( 'NONE', #10435, 26.00000000000000355 ) ;
#12959 = DIRECTION ( 'NONE',  ( 0.000000000000000000, 0.000000000000000000, 1.000000000000000000 ) ) ;
#12960 = DIRECTION ( 'NONE',  ( -0.000000000000000000, 1.000000000000000000, -0.000000000000000000 ) ) ;
#12961 = DIRECTION ( 'NONE',  ( 0.000000000000000000, -0.000000000000000000, 1.000000000000000000 ) ) ;
#12962 = CARTESIAN_POINT ( 'NONE',  ( -15.58845726811999910, 7.773118517290098950, 10.99999999999985256 ) ) ;
#12963 = CARTESIAN_POINT ( 'NONE',  ( 2.443868322553949479, 71.76788406128898146, 13.27695547668219866 ) ) ;
#12964 = CARTESIAN_POINT ( 'NONE',  ( 13.50000000000000355, 54.57999999999999119, -4.386415899144233244 ) ) ;
#12965 = CARTESIAN_POINT ( 'NONE',  ( -0.4388680196204213790, 71.66422011136278059, 13.49292316262332214 ) ) ;
#12966 = CARTESIAN_POINT ( 'NONE',  ( 18.62500000000000000, -99.89999999999976410, 0.000000000000000000 ) ) ;
#12967 = VECTOR ( 'NONE', #14585, 1000.000000000000000 ) ;
#12968 = CARTESIAN_POINT ( 'NONE',  ( -7.714727599200467800, -78.04687499999982947, 18.62499999999934630 ) ) ;
#12969 = CARTESIAN_POINT ( 'NONE',  ( -11.63268444319199624, 68.18495566772109839, 6.850846920013293762 ) ) ;
#12970 = CARTESIAN_POINT ( 'NONE',  ( 18.62500000000064304, -67.64062499999984368, -7.714727599197335195 ) ) ;
#12971 = CARTESIAN_POINT ( 'NONE',  ( 5.390530401168515340, 54.98489645169363627, -12.37944730132690196 ) ) ;
#12972 = CARTESIAN_POINT ( 'NONE',  ( -18.62500000000000000, -41.62499999999990052, -1.562973063126292555E-12 ) ) ;
#12973 = CARTESIAN_POINT ( 'NONE',  ( 8.549612433556128696E-08, 65.68000242247177312, 13.49999999999999822 ) ) ;
#12974 = CARTESIAN_POINT ( 'NONE',  ( 12.00000000000000178, 8.146025403784442176, 3.899036354794877202 ) ) ;
#12975 = CARTESIAN_POINT ( 'NONE',  ( -11.21669893531349160, 35.21226868908650687, 7.512399413318213703 ) ) ;
#12976 = CARTESIAN_POINT ( 'NONE',  ( -10.92172942406178926, 23.63000000000001322, -7.935100905948389460 ) ) ;
#12977 = VERTEX_POINT ( 'NONE', #8344 ) ;
#12978 = CARTESIAN_POINT ( 'NONE',  ( -11.76794919243112325, 32.92999999999999972, -2.882316262207890869E-15 ) ) ;
#12979 = CARTESIAN_POINT ( 'NONE',  ( -5.257100738639275406, 40.37012037508893769, -12.43485227326261011 ) ) ;
#12980 = CARTESIAN_POINT ( 'NONE',  ( -11.86009848853153947, 31.69125030478712191, -6.448902088085707973 ) ) ;
#12981 = FACE_BOUND ( 'NONE', #15131, .T. ) ;
#12982 = CARTESIAN_POINT ( 'NONE',  ( 11.88531977884646196, 60.19299833890768525, 6.407369536219499118 ) ) ;
#12983 = CARTESIAN_POINT ( 'NONE',  ( 8.343458848123578520, -2.020000000000003126, 11.48378591275254124 ) ) ;
#12984 = CARTESIAN_POINT ( 'NONE',  ( 4.178864255851000829E-14, 61.67999999999999261, 13.50000000000000000 ) ) ;
#12985 = ADVANCED_FACE ( 'NONE', ( #370 ), #8522, .F. ) ;
#12986 = CARTESIAN_POINT ( 'NONE',  ( 4.171729424061789260, 73.83000000000001251, 12.83926296998457417 ) ) ;
#12987 = CARTESIAN_POINT ( 'NONE',  ( 12.05091702511513851, 51.65458203422696926, -6.096857118557952759 ) ) ;
#12988 = CARTESIAN_POINT ( 'NONE',  ( -10.33299960000793050, 38.26336937052408871, 8.690946034728787239 ) ) ;
#12989 = CARTESIAN_POINT ( 'NONE',  ( 13.04240740954509015, 36.55426163316852239, -3.485073724549926588 ) ) ;
#12990 = CARTESIAN_POINT ( 'NONE',  ( -11.37499999999960210, -47.83437499999990195, -4.711679271994911211 ) ) ;
#12991 = CARTESIAN_POINT ( 'NONE',  ( 12.00000000000000355, 2.446025403784435337, -3.899036354794874093 ) ) ;
#12992 =( BOUNDED_CURVE ( )  B_SPLINE_CURVE ( 2, ( #13609, #14925, #9403, #10976, #13691, #1323, #9575, #8335, #7, #7007, #190, #17414, #15994 ),
 .UNSPECIFIED., .F., .F. ) 
 B_SPLINE_CURVE_WITH_KNOTS ( ( 3, 2, 2, 2, 2, 2, 3 ),
 ( 0.5416666666666666297, 0.5444444444444443976, 0.5500000000000000444, 0.5555555555555555802, 0.5611111111111111160, 0.5666666666666666519, 0.5694444444444444198 ),
 .UNSPECIFIED. ) 
 CURVE ( )  GEOMETRIC_REPRESENTATION_ITEM ( )  RATIONAL_B_SPLINE_CURVE ( ( 0.9755282581475768211, 0.9755282581475768211, 1.000000000000000000, 0.9510565162951535312, 1.000000000000000000, 0.9510565162951535312, 1.000000000000000000, 0.9510565162951535312, 1.000000000000000000, 0.9510565162951535312, 1.000000000000000000, 0.9755282581475768211, 0.9755282581475768211 ) ) 
 REPRESENTATION_ITEM ( '' )  );
#12993 = CARTESIAN_POINT ( 'NONE',  ( -10.79460918060730990, 77.23732893913023645, 8.107729363714126336 ) ) ;
#12994 = CARTESIAN_POINT ( 'NONE',  ( -3.066993958782973095, 80.56964720549299841, 13.15436491285448106 ) ) ;
#12995 = CARTESIAN_POINT ( 'NONE',  ( 3.833221879840224222, 41.81748144897261454, 12.94619382350246184 ) ) ;
#12996 = ORIENTED_EDGE ( 'NONE', *, *, #14449, .T. ) ;
#12997 = CARTESIAN_POINT ( 'NONE',  ( 9.520470885617715595, 14.13000000000000433, 6.917026985038135400 ) ) ;
#12998 = CARTESIAN_POINT ( 'NONE',  ( 0.000000000000000000, 30.93000000000001393, 0.000000000000000000 ) ) ;
#12999 = ORIENTED_EDGE ( 'NONE', *, *, #5035, .T. ) ;
#13000 = CARTESIAN_POINT ( 'NONE',  ( -7.576616670048093940E-16, 57.67999999999999261, 12.37355403259654807 ) ) ;
#13001 = CARTESIAN_POINT ( 'NONE',  ( 8.043339635997652337, -44.78124999999987921, -8.043339635996304082 ) ) ;
#13002 = DIRECTION ( 'NONE',  ( 0.000000000000000000, -1.000000000000000000, 0.000000000000000000 ) ) ;
#13003 = CARTESIAN_POINT ( 'NONE',  ( 2.150159292860549076, 80.92999999999997840, -13.03677673010519733 ) ) ;
#13004 = CARTESIAN_POINT ( 'NONE',  ( 18.62500000000000000, -83.24999999999980105, 1.560692158462880521E-12 ) ) ;
#13005 =( GEOMETRIC_REPRESENTATION_CONTEXT ( 3 ) GLOBAL_UNCERTAINTY_ASSIGNED_CONTEXT ( ( #16690 ) ) GLOBAL_UNIT_ASSIGNED_CONTEXT ( ( #13772, #15356, #868 ) ) REPRESENTATION_CONTEXT ( 'NONE', 'WORKASPACE' ) );
#13006 = CARTESIAN_POINT ( 'NONE',  ( -8.343458848123576743, 82.47999999999997556, -11.48378591275254301 ) ) ;
#13007 = EDGE_CURVE ( 'NONE', #5466, #8460, #16134, .T. ) ;
#13008 = CARTESIAN_POINT ( 'NONE',  ( -7.272992578804307939, 50.47999999999999687, -10.01041549318726886 ) ) ;
#13009 = DIRECTION ( 'NONE',  ( 0.000000000000000000, 0.000000000000000000, -1.000000000000000000 ) ) ;
#13010 = CARTESIAN_POINT ( 'NONE',  ( -11.20034620794313440, 59.21330483900249675, 7.537432996273548014 ) ) ;
#13011 = B_SPLINE_CURVE_WITH_KNOTS ( 'NONE', 3,
 ( #5118, #2850, #3779, #15872, #2761, #12421, #13642, #41, #5446, #15046, #2941, #132, #12240, #9191, #8193, #1536, #4377, #13555, #15132, #8370, #8105, #10833, #16195, #7043, #4107, #1446, #308, #5538, #16291, #13727, #9609, #12329, #13470, #224, #11011, #16382, #1625, #5717, #9785, #7776, #13149, #1037, #1712, #16562, #12593, #569, #14161, #1795, #11271, #7125, #742, #11187, #1879, #3303, #7294, #15223, #9959, #5976, #7473, #10046, #8716, #8459, #3029, #15307, #1963, #16648, #6062, #4469, #8632, #11358, #484, #16907, #5892, #16818, #13983, #10212, #12764, #7386, #13813, #7207, #4555, #396, #12511, #11445, #3212, #5803, #9874, #4810, #652, #3121, #4726, #8547, #10127, #13898, #2049, #12679, #11529, #15480, #3391, #8804, #16732, #4639, #12853, #15395, #14076, #6152, #7731, #13022, #14245, #11701, #3826, #2303, #14501, #16992, #10297, #819, #17253, #11790, #4897, #15832, #14415, #14329, #14594, #15917, #17167, #9240, #3648, #3476, #15565, #4982, #2388, #17078, #1082, #15649, #9062, #13107, #7645, #11962, #904, #11878, #994, #6406, #5077, #8890, #2130, #10471, #7556, #12935, #5252, #6495, #10385, #6230, #11617, #17341, #7824, #3559, #5166, #8973, #10558, #2218, #2474, #3737, #15739, #6315, #9154, #7907, #13196, #13282, #1170, #6581, #17423, #10638, #5338, #10723, #13362, #9412 ),
 .UNSPECIFIED., .F., .F.,
 ( 4, 2, 2, 1, 2, 2, 1, 2, 2, 1, 2, 2, 1, 1, 2, 2, 2, 1, 2, 2, 2, 2, 2, 2, 2, 2, 1, 1, 1, 2, 2, 1, 1, 1, 2, 2, 2, 2, 2, 2, 2, 1, 2, 2, 2, 2, 2, 2, 1, 1, 1, 2, 1, 2, 2, 1, 1, 2, 2, 2, 1, 1, 1, 1, 2, 2, 2, 2, 2, 2, 2, 1, 2, 2, 1, 2, 2, 2, 2, 2, 2, 2, 1, 2, 2, 2, 1, 2, 2, 1, 2, 2, 2, 2, 1, 2, 2, 1, 2, 2, 2, 2, 4 ),
 ( 0.3578158167825879477, 0.3587362859346358013, 0.3591965205106597558, 0.3593115791546657722, 0.3593691084766687527, 0.3593978731376702429, 0.3594266377986717331, 0.3596567550866837104, 0.3605772242387316195, 0.3606059888997331098, 0.3606203712302338271, 0.3606347535607346000, 0.3606922828827375804, 0.3608073415267435968, 0.3610374588147555741, 0.3614976933907795287, 0.3617278106787915060, 0.3618428693227974668, 0.3618716339837989571, 0.3619003986448004473, 0.3619579279668034832, 0.3624181625428274378, 0.3633386316948752914, 0.3642591008469232006, 0.3643741594909292170, 0.3644029241519307072, 0.3644316888129321974, 0.3644892181349351779, 0.3647193354229471551, 0.3651795699989711652, 0.3661000391510190743, 0.3665602737270430289, 0.3667903910150550617, 0.3668479203370580422, 0.3668766849980595324, 0.3669054496590610226, 0.3670205083030670390, 0.3688614466071628017, 0.3693216811831867008, 0.3693792105051897368, 0.3694367398271927172, 0.3695517984711986781, 0.3697819157592106554, 0.3707023849112585645, 0.3716228540633064181, 0.3718529713513183954, 0.3718817360123198856, 0.3719105006733214314, 0.3719680299953244118, 0.3720830886393303727, 0.3725433232153543273, 0.3730035577913782818, 0.3731186164353842982, 0.3731329987658850156, 0.3731473810963857884, 0.3731761457573872787, 0.3732336750793902591, 0.3734637923674022364, 0.3743842615194501455, 0.3744130261804516357, 0.3744417908414531260, 0.3744993201634561619, 0.3746143788074621228, 0.3748444960954741001, 0.3753047306714980547, 0.3762251998235459638, 0.3766854343995698629, 0.3768004930435758792, 0.3769155516875818401, 0.3771456689755938174, 0.3780661381276417266, 0.3781236674496447070, 0.3781380497801454799, 0.3781524321106461972, 0.3781811967716476874, 0.3782962554156537038, 0.3785263727036656811, 0.3789866072796896912, 0.3792167245677016685, 0.3793317832117076849, 0.3793893125337106653, 0.3794180771947121555, 0.3794468418557136458, 0.3799070764317378224, 0.3808275455837860646, 0.3817480147358343623, 0.3818630733798403787, 0.3818918380408418689, 0.3819206027018434146, 0.3819781320238463951, 0.3822082493118584834, 0.3826684838878826600, 0.3835889530399310132, 0.3840491876159551898, 0.3842793049039672226, 0.3843943635479732945, 0.3844231282089747848, 0.3844518928699763305, 0.3845094221919793109, 0.3854298913440276086, 0.3863503604960759064, 0.3868105950721000275, 0.3872708296481242041 ),
 .UNSPECIFIED. ) ;
#13012 = CARTESIAN_POINT ( 'NONE',  ( 10.47861606810065815, 45.10486826704778451, 8.511906612892380153 ) ) ;
#13013 = CARTESIAN_POINT ( 'NONE',  ( 11.94609836220409349, 69.66229794021633381, -6.288142491076607499 ) ) ;
#13014 = DIRECTION ( 'NONE',  ( 0.5000000000000104361, 0.000000000000000000, -0.8660254037844326014 ) ) ;
#13015 = CARTESIAN_POINT ( 'NONE',  ( 11.77408743055708662, 30.67508156744361969, -6.605444128499801337 ) ) ;
#13016 = CARTESIAN_POINT ( 'NONE',  ( -10.98298365945945143, 56.22644425589727035, 7.850925719499952216 ) ) ;
#13017 = CARTESIAN_POINT ( 'NONE',  ( -5.569062747661596369, 50.47790839199158341, 12.29782247994843658 ) ) ;
#13018 = CARTESIAN_POINT ( 'NONE',  ( 15.58845726811991916, 7.773118517290098950, -10.99999999999996092 ) ) ;
#13019 = CARTESIAN_POINT ( 'NONE',  ( 2.530352284268557295, 43.08905591751716457, -13.26307597662109927 ) ) ;
#13020 = CARTESIAN_POINT ( 'NONE',  ( 7.498839979050778481, 39.89913384926502005, -11.22908298276431260 ) ) ;
#13021 = EDGE_LOOP ( 'NONE', ( #4899, #4788, #1104, #3673, #8034, #9035, #7650, #14137, #570, #6517 ) ) ;
#13022 = CARTESIAN_POINT ( 'NONE',  ( -12.64888242172768607, 61.75875439202012274, -4.738583482749483267 ) ) ;
#13023 = CARTESIAN_POINT ( 'NONE',  ( 9.520470885617715595, 8.129999999999999005, 6.917026985038135400 ) ) ;
#13024 = ORIENTED_EDGE ( 'NONE', *, *, #3626, .T. ) ;
#13025 = CARTESIAN_POINT ( 'NONE',  ( -8.571272707445116268, 40.50886853748669836, -10.43127125671136568 ) ) ;
#13026 = ORIENTED_EDGE ( 'NONE', *, *, #2873, .F. ) ;
#13027 = CARTESIAN_POINT ( 'NONE',  ( 2.621994543952811015E-15, 34.18000000000000682, -14.19474002721660355 ) ) ;
#13028 = CARTESIAN_POINT ( 'NONE',  ( -13.16986379960055231, -10.40624999999997513, 13.16986379959834252 ) ) ;
#13029 = CARTESIAN_POINT ( 'NONE',  ( 6.014033562793300369, 47.89924598142680878, 12.09241346544142104 ) ) ;
#13030 = CARTESIAN_POINT ( 'NONE',  ( 11.16378927044967462, 57.71547821250464949, -7.596269605373482392 ) ) ;
#13031 = CARTESIAN_POINT ( 'NONE',  ( 6.974580545495159711, 78.92141596235254042, -11.55926377139148897 ) ) ;
#13032 = CARTESIAN_POINT ( 'NONE',  ( -11.76794919243112325, 80.78000000000000114, -3.823638476888998827 ) ) ;
#13033 = CARTESIAN_POINT ( 'NONE',  ( 11.76794919243112325, 82.27999999999998693, 3.823638476888996607 ) ) ;
#13034 = ADVANCED_FACE ( 'NONE', ( #15103 ), #6837, .F. ) ;
#13035 = DIRECTION ( 'NONE',  ( 0.000000000000000000, 1.000000000000000000, 0.000000000000000000 ) ) ;
#13036 = B_SPLINE_CURVE_WITH_KNOTS ( 'NONE', 3,
 ( #1690, #8172, #6931, #16359, #13535, #3007, #5518, #7105, #203, #9763, #1605, #11078, #16271, #6842, #7021, #16630, #2831, #13791, #1425, #12400, #9676, #12489, #4447, #12309, #4177, #5609, #11165, #11251, #8262, #4354, #8437, #4266, #12218, #15026, #8528, #288, #374, #9589, #14939, #10900, #9854, #1778, #13622, #5780 ),
 .UNSPECIFIED., .F., .F.,
 ( 4, 2, 2, 2, 2, 2, 2, 2, 2, 2, 2, 2, 2, 2, 2, 2, 2, 2, 2, 2, 2, 4 ),
 ( 0.03689401835950767428, 0.03766257893388839234, 0.03843113950826911041, 0.03919970008264983541, 0.03996826065703055347, 0.04073682123141127154, 0.04150538180579199654, 0.04304250295455346043, 0.04457962410331493125, 0.04611674525207640207, 0.04765386640083786596, 0.04919098754959933678, 0.05072810869836080067, 0.05226522984712227149, 0.05380235099588373537, 0.05533947214464519926, 0.05687659329340666314, 0.05764515386778738815, 0.05841371444216810621, 0.05995083559092950765, 0.06071939616531019102, 0.06148795673969087439 ),
 .UNSPECIFIED. ) ;
#13037 = CARTESIAN_POINT ( 'NONE',  ( 13.50000000000000000, 41.42999999999999972, 1.653273178848926867E-15 ) ) ;
#13038 = DIRECTION ( 'NONE',  ( 0.000000000000000000, -0.000000000000000000, -1.000000000000000000 ) ) ;
#13039 = CARTESIAN_POINT ( 'NONE',  ( 11.37500000000039613, -60.39062499999985079, -4.711679271993004292 ) ) ;
#13040 = CARTESIAN_POINT ( 'NONE',  ( -7.499999999999996447, -21.99999999999990052, 9.367496997597656971 ) ) ;
#13041 = CARTESIAN_POINT ( 'NONE',  ( 5.544738967689208486, 33.97889555847616094, -12.31101044224262253 ) ) ;
#13042 = ORIENTED_EDGE ( 'NONE', *, *, #8177, .T. ) ;
#13043 = DIRECTION ( 'NONE',  ( 0.000000000000000000, -0.000000000000000000, -1.000000000000000000 ) ) ;
#13044 = VERTEX_POINT ( 'NONE', #12484 ) ;
#13045 = AXIS2_PLACEMENT_3D ( 'NONE', #884, #9133, #14482 ) ;
#13046 = CARTESIAN_POINT ( 'NONE',  ( -13.49999999999999822, 16.78000000000001535, -4.386415899144240349 ) ) ;
#13047 = CARTESIAN_POINT ( 'NONE',  ( -4.711679271993001628, -29.10312499999994884, -11.37500000000039613 ) ) ;
#13048 = CARTESIAN_POINT ( 'NONE',  ( 0.8898902232607978080, 77.71204398683455850, 13.47798471056508873 ) ) ;
#13049 = CARTESIAN_POINT ( 'NONE',  ( -3.352402354136216900, 59.55948517377429852, 13.07833649419892730 ) ) ;
#13050 = CARTESIAN_POINT ( 'NONE',  ( -8.891200544363830713E-16, 1.546025403784439423, 12.00000000000000000 ) ) ;
#13051 = CARTESIAN_POINT ( 'NONE',  ( -18.06260399879761636, 6.548267719634618622, 15.28534784291383986 ) ) ;
#13052 = CARTESIAN_POINT ( 'NONE',  ( -8.343458848123582072, 56.38000000000000256, 11.48378591275254124 ) ) ;
#13053 = CARTESIAN_POINT ( 'NONE',  ( -6.097425033090877911, 71.45719859721984335, 12.04586506600376161 ) ) ;
#13054 = AXIS2_PLACEMENT_3D ( 'NONE', #16172, #7016, #16 ) ;
#13055 = CYLINDRICAL_SURFACE ( 'NONE', #12946, 1.999999999999997335 ) ;
#13056 = CARTESIAN_POINT ( 'NONE',  ( 13.16986379960055054, -85.33124999999978400, -13.16986379959834430 ) ) ;
#13057 = CARTESIAN_POINT ( 'NONE',  ( 3.045871263339404056, 68.78958672362097104, 13.15403766504849159 ) ) ;
#13058 = CARTESIAN_POINT ( 'NONE',  ( -18.62500000000064659, -42.66562499999989200, 7.714727599197335195 ) ) ;
#13059 = CARTESIAN_POINT ( 'NONE',  ( 3.169521232131934596, 55.06603785773634741, -13.12275766666495613 ) ) ;
#13060 = CARTESIAN_POINT ( 'NONE',  ( -18.62499999999934985, -7.284374999999982947, -7.714727599200458918 ) ) ;
#13061 = CARTESIAN_POINT ( 'NONE',  ( -6.285214426531775977, 65.44986835950689397, 11.95462813086504106 ) ) ;
#13062 = CARTESIAN_POINT ( 'NONE',  ( 10.84916736553044991, 7.815485454866775150, -15.50137400600630144 ) ) ;
#13063 = CARTESIAN_POINT ( 'NONE',  ( -11.25052883642759483, 35.21015491215516136, 7.461608953425876045 ) ) ;
#13064 = CARTESIAN_POINT ( 'NONE',  ( 11.76794919243112325, 31.42999999999999972, 1.441158131103945434E-15 ) ) ;
#13065 = CARTESIAN_POINT ( 'NONE',  ( -5.521256578040511620, 40.38024479432580449, -12.31935789223439492 ) ) ;
#13066 = AXIS2_PLACEMENT_3D ( 'NONE', #7164, #346, #12369 ) ;
#13067 = CARTESIAN_POINT ( 'NONE',  ( -13.48148663984154894, 31.90541497078363520, -0.7088848451981341059 ) ) ;
#13068 = CARTESIAN_POINT ( 'NONE',  ( 7.999999999999850786, 5.918584287042170544, 24.73863375370601858 ) ) ;
#13069 = CARTESIAN_POINT ( 'NONE',  ( 11.72855914400952315, 60.18170760815687714, 6.685430133444309142 ) ) ;
#13070 = CARTESIAN_POINT ( 'NONE',  ( -8.343458848123582072, -8.619999999999997442, 11.48378591275254124 ) ) ;
#13071 = CARTESIAN_POINT ( 'NONE',  ( -7.148322466681692688, 53.41409683114213891, 11.45214043970867301 ) ) ;
#13072 = CARTESIAN_POINT ( 'NONE',  ( -11.76794919243112325, 56.92999999999999972, -2.882316262207890869E-15 ) ) ;
#13073 = CARTESIAN_POINT ( 'NONE',  ( 13.40257667448758916, 51.37355437458653995, 1.618959382087582721 ) ) ;
#13074 = CARTESIAN_POINT ( 'NONE',  ( -13.47552119200681808, 37.90193867599817423, -0.8126124652662984893 ) ) ;
#13075 = CARTESIAN_POINT ( 'NONE',  ( 13.05049472663724330, 36.55313275038592025, -3.454688345068896105 ) ) ;
#13076 = CARTESIAN_POINT ( 'NONE',  ( 8.043339635997652337, -25.98124999999995310, -8.043339635996302306 ) ) ;
#13077 = CARTESIAN_POINT ( 'NONE',  ( -8.891200544363830713E-16, 1.546025403784439423, 12.00000000000000000 ) ) ;
#13078 = CARTESIAN_POINT ( 'NONE',  ( -4.945268273999643860, 77.50155154180465900, 12.56911554149012922 ) ) ;
#13079 = CARTESIAN_POINT ( 'NONE',  ( 4.299690572160308814E-08, 62.68000119825558869, 13.49999999999999822 ) ) ;
#13080 = CARTESIAN_POINT ( 'NONE',  ( 0.000000000000000000, 102.9300000000000068, -12.00000000000000178 ) ) ;
#13081 = ORIENTED_EDGE ( 'NONE', *, *, #9524, .T. ) ;
#13082 = CARTESIAN_POINT ( 'NONE',  ( -9.520470885617715595, 12.63000000000000256, -6.917026985038136289 ) ) ;
#13083 = CARTESIAN_POINT ( 'NONE',  ( 0.000000000000000000, 9.000000000000000000, -12.00000000000000178 ) ) ;
#13084 = EDGE_CURVE ( 'NONE', #8166, #1252, #13326, .T. ) ;
#13085 = ORIENTED_EDGE ( 'NONE', *, *, #17130, .F. ) ;
#13086 = CARTESIAN_POINT ( 'NONE',  ( -9.520470885617717371, 60.22999999999999687, 6.917026985038133624 ) ) ;
#13087 = CARTESIAN_POINT ( 'NONE',  ( 8.043339635996302306, -57.26874999999984794, 8.043339635997654113 ) ) ;
#13088 = CARTESIAN_POINT ( 'NONE',  ( 8.000000000000021316, 7.170682760640493036, -19.79706521687766596 ) ) ;
#13089 = CARTESIAN_POINT ( 'NONE',  ( -13.50000000000000000, 1.930000000000015037, -3.469446951953614189E-15 ) ) ;
#13090 = CARTESIAN_POINT ( 'NONE',  ( 8.252097576776698418, 75.86575466930307243, -10.68462399792931805 ) ) ;
#13091 = CARTESIAN_POINT ( 'NONE',  ( 7.714727599197339636, -63.47812499999984226, 18.62500000000063949 ) ) ;
#13092 = CARTESIAN_POINT ( 'NONE',  ( 2.607531440858944223E-15, 73.17999999999999261, -14.19474002721660355 ) ) ;
#13093 = CARTESIAN_POINT ( 'NONE',  ( 2.272985001014427788E-15, 47.17999999999999972, -12.37355403259654985 ) ) ;
#13094 = CARTESIAN_POINT ( 'NONE',  ( 12.50000000000000000, -18.00000000000000355, -2.204364238465235822E-15 ) ) ;
#13095 = CARTESIAN_POINT ( 'NONE',  ( -13.46060157357587705, 58.96570155535383861, 1.031214257062757156 ) ) ;
#13096 = CARTESIAN_POINT ( 'NONE',  ( 13.48827146342498118, 45.41039300781007171, 0.5693795367556682141 ) ) ;
#13097 = CARTESIAN_POINT ( 'NONE',  ( 10.26325473544014244, 69.76683747837135741, -8.770540033709549377 ) ) ;
#13098 = CARTESIAN_POINT ( 'NONE',  ( 1.651742348007693817, 80.73938956827036861, 13.39882440897573090 ) ) ;
#13099 = CARTESIAN_POINT ( 'NONE',  ( 13.19255495532672384, 30.32843427499656741, 2.870686787867847922 ) ) ;
#13100 = CARTESIAN_POINT ( 'NONE',  ( -9.894286701644787740, 55.57365333309054733, -9.185706287943689929 ) ) ;
#13101 = CARTESIAN_POINT ( 'NONE',  ( -13.44902317320591223, 49.97066846970101039, 1.172593465884237185 ) ) ;
#13102 = DIRECTION ( 'NONE',  ( 0.5000000000000012212, 0.000000000000000000, -0.8660254037844379305 ) ) ;
#13103 = CARTESIAN_POINT ( 'NONE',  ( 13.02724366109965359, 42.55636079357457646, -3.541529992081969169 ) ) ;
#13104 = CARTESIAN_POINT ( 'NONE',  ( 12.73078937444389958, 39.26766722070165372, 4.496366551774039877 ) ) ;
#13105 = EDGE_LOOP ( 'NONE', ( #16623, #1084, #2851, #2760 ) ) ;
#13106 = CARTESIAN_POINT ( 'NONE',  ( -12.78543602905191356, 70.77384588509148955, -4.334193518847205162 ) ) ;
#13107 = CARTESIAN_POINT ( 'NONE',  ( -10.07944169913838550, 61.58339775250015435, -8.980808011171538041 ) ) ;
#13108 = CARTESIAN_POINT ( 'NONE',  ( -11.76794919243112325, 3.780000000000002913, -3.823638476888998827 ) ) ;
#13109 = EDGE_LOOP ( 'NONE', ( #13285, #2782, #992, #14782, #12999, #628 ) ) ;
#13110 = CARTESIAN_POINT ( 'NONE',  ( -10.31701163439258195, 40.59603470620067611, -8.706927762819312022 ) ) ;
#13111 = ORIENTED_EDGE ( 'NONE', *, *, #14898, .T. ) ;
#13112 = CARTESIAN_POINT ( 'NONE',  ( -8.343458848123576743, 25.48000000000001819, -11.48378591275254301 ) ) ;
#13113 = CARTESIAN_POINT ( 'NONE',  ( -7.714727599200467800, -94.69687499999979252, 18.62499999999934630 ) ) ;
#13114 = CARTESIAN_POINT ( 'NONE',  ( -9.999999999999776179, 0.000000000000000000, -15.32050807568890605 ) ) ;
#13115 = DIRECTION ( 'NONE',  ( 0.000000000000000000, 0.000000000000000000, -1.000000000000000000 ) ) ;
#13116 = CARTESIAN_POINT ( 'NONE',  ( 12.19413841524875686, 78.64259250466695050, -5.792494143745500423 ) ) ;
#13117 = CARTESIAN_POINT ( 'NONE',  ( -7.272992578804307939, 80.48000000000000398, -10.01041549318726886 ) ) ;
#13118 = CARTESIAN_POINT ( 'NONE',  ( -11.76794919243112325, 83.93000000000000682, -2.882316262207890869E-15 ) ) ;
#13119 = CARTESIAN_POINT ( 'NONE',  ( 0.000000000000000000, 80.93000000000000682, 0.000000000000000000 ) ) ;
#13120 = CARTESIAN_POINT ( 'NONE',  ( 10.73134851898655917, -99.99999999999995737, 4.282261568526099182 ) ) ;
#13121 = PLANE ( 'NONE',  #17276 ) ;
#13122 = CARTESIAN_POINT ( 'NONE',  ( 11.37500000000039613, -77.04062499999979252, -4.711679271993004292 ) ) ;
#13123 = DIRECTION ( 'NONE',  ( -1.000000000000000000, -0.000000000000000000, -0.000000000000000000 ) ) ;
#13124 = CARTESIAN_POINT ( 'NONE',  ( 9.380613467790862359, 33.81254506432511420, -9.717859427143588746 ) ) ;
#13125 = CARTESIAN_POINT ( 'NONE',  ( -13.41322977063805411, 73.87657456906511300, -1.534601281563461317 ) ) ;
#13126 = ORIENTED_EDGE ( 'NONE', *, *, #7375, .F. ) ;
#13127 = EDGE_CURVE ( 'NONE', #14678, #12894, #6809, .T. ) ;
#13128 = VERTEX_POINT ( 'NONE', #9774 ) ;
#13129 = LINE ( 'NONE', #11547, #14574 ) ;
#13130 = EDGE_CURVE ( 'NONE', #11984, #1191, #7419, .T. ) ;
#13131 = VERTEX_POINT ( 'NONE', #6942 ) ;
#13132 = CARTESIAN_POINT ( 'NONE',  ( -13.49999999999999822, 13.78000000000000824, -4.386415899144240349 ) ) ;
#13133 = CARTESIAN_POINT ( 'NONE',  ( 4.711679271993006957, -20.77812499999997087, 11.37500000000039257 ) ) ;
#13134 = CARTESIAN_POINT ( 'NONE',  ( -5.485275766071775660E-07, 44.67998473833578998, 13.49999999999997691 ) ) ;
#13135 = FACE_OUTER_BOUND ( 'NONE', #397, .T. ) ;
#13136 = DIRECTION ( 'NONE',  ( 9.637352644315600173E-17, -1.000000000000000000, 0.000000000000000000 ) ) ;
#13137 = CARTESIAN_POINT ( 'NONE',  ( 11.61487935108414860, 66.68628431109220855, -6.880802064610810120 ) ) ;
#13138 = CARTESIAN_POINT ( 'NONE',  ( -10.92172942406178926, 52.62999999999999545, -7.935100905948389460 ) ) ;
#13139 = CARTESIAN_POINT ( 'NONE',  ( -5.359544901455636001, 71.48597326161704757, 12.39102907241780827 ) ) ;
#13140 = VECTOR ( 'NONE', #9301, 1000.000000000000000 ) ;
#13141 = CARTESIAN_POINT ( 'NONE',  ( -18.62500000000000000, -1.074999999999978639, -1.562973063126292757E-12 ) ) ;
#13142 = CARTESIAN_POINT ( 'NONE',  ( 2.924053257345435538E-06, 68.68008145904181561, 13.49999999999936584 ) ) ;
#13143 = CARTESIAN_POINT ( 'NONE',  ( -18.62499999999934985, -57.23437499999987921, -7.714727599200458918 ) ) ;
#13144 = CARTESIAN_POINT ( 'NONE',  ( 6.308629901301857856, 54.94873493297386347, -11.93532085539004051 ) ) ;
#13145 = CARTESIAN_POINT ( 'NONE',  ( 11.76794919243112325, 20.43000000000000327, 1.734723475976807094E-15 ) ) ;
#13146 = CARTESIAN_POINT ( 'NONE',  ( 18.62500000000064304, -67.64062499999984368, -7.714727599197335195 ) ) ;
#13147 = CARTESIAN_POINT ( 'NONE',  ( -2.514869812877075006, 65.58957455577544238, 13.26368900418464492 ) ) ;
#13148 = EDGE_CURVE ( 'NONE', #2258, #8561, #14951, .T. ) ;
#13149 = CARTESIAN_POINT ( 'NONE',  ( -7.881676343575944266, 62.38282404488849409, 10.98390370778267311 ) ) ;
#13150 = CARTESIAN_POINT ( 'NONE',  ( -1.388180886794196711, 35.63013967225546708, 13.42855345809681289 ) ) ;
#13151 = ORIENTED_EDGE ( 'NONE', *, *, #773, .F. ) ;
#13152 = CARTESIAN_POINT ( 'NONE',  ( -15.58845726811999910, 0.000000000000000000, 10.99999999999985256 ) ) ;
#13153 = COLOUR_RGB ( '',0.7921568627450980005, 0.8196078431372548767, 0.9333333333333333481 ) ;
#13154 = CARTESIAN_POINT ( 'NONE',  ( -13.47846937990238914, 31.96028432000488095, 0.8791170498727822746 ) ) ;
#13155 = CARTESIAN_POINT ( 'NONE',  ( 0.4269699266103727520, 73.16464788207684933, -13.49334228634718258 ) ) ;
#13156 = CARTESIAN_POINT ( 'NONE',  ( 9.324401936112977296, 60.04491477143539413, 9.762614344302546598 ) ) ;
#13157 = CARTESIAN_POINT ( 'NONE',  ( -8.343458848123576743, -6.520000000000006679, -11.48378591275254301 ) ) ;
#13158 = CARTESIAN_POINT ( 'NONE',  ( -0.5897042632328444167, 53.65879917600137361, 13.48805907082272704 ) ) ;
#13159 = CARTESIAN_POINT ( 'NONE',  ( -9.520470885617717371, 54.23000000000000398, 6.917026985038133624 ) ) ;
#13160 = CARTESIAN_POINT ( 'NONE',  ( 13.22767550596827313, 51.52528944818870116, -2.697998014972899927 ) ) ;
#13161 = CIRCLE ( 'NONE', #15689, 1.999999999999998224 ) ;
#13162 = CARTESIAN_POINT ( 'NONE',  ( -11.13964547656885706, 38.21702771554652855, 7.626358909834451971 ) ) ;
#13163 = CARTESIAN_POINT ( 'NONE',  ( 13.49038636612923803, 36.44758377910591207, -0.5111530726713751083 ) ) ;
#13164 = CARTESIAN_POINT ( 'NONE',  ( 4.711679271994911211, -43.67187499999991473, -11.37499999999960210 ) ) ;
#13165 = CARTESIAN_POINT ( 'NONE',  ( 7.416407864998740607, 2.746025403784439600, -10.20780970022447676 ) ) ;
#13166 = CARTESIAN_POINT ( 'NONE',  ( -10.66896271836897725, 77.24446959830603987, 8.271838784292951274 ) ) ;
#13167 = EDGE_CURVE ( 'NONE', #7861, #1880, #7702, .T. ) ;
#13168 = CARTESIAN_POINT ( 'NONE',  ( 2.435030327634469582, 62.76764002089962702, 13.27876764330338588 ) ) ;
#13169 = CARTESIAN_POINT ( 'NONE',  ( 7.500000000000000000, 103.9536021580775014, -9.261711852864907613 ) ) ;
#13170 = VERTEX_POINT ( 'NONE', #2751 ) ;
#13171 = CARTESIAN_POINT ( 'NONE',  ( 11.76794919243112325, 11.42999999999999616, 1.734723475976807094E-15 ) ) ;
#13172 = ORIENTED_EDGE ( 'NONE', *, *, #11201, .F. ) ;
#13173 = CARTESIAN_POINT ( 'NONE',  ( 7.272992578804311492, 58.88000000000000256, -10.01041549318726886 ) ) ;
#13174 = CARTESIAN_POINT ( 'NONE',  ( -4.711679271994916540, -87.44687499999976410, 11.37499999999960565 ) ) ;
#13175 = CARTESIAN_POINT ( 'NONE',  ( 8.375056734751542109, 9.999950376471138824, 10.58801762894534271 ) ) ;
#13176 = CARTESIAN_POINT ( 'NONE',  ( 10.92172942406178926, 0.1300000000000051115, 7.935100905948385908 ) ) ;
#13177 = CARTESIAN_POINT ( 'NONE',  ( 8.496523779928633502, 75.85456680855661205, -10.49111029357017344 ) ) ;
#13178 = AXIS2_PLACEMENT_3D ( 'NONE', #9085, #14263, #4917 ) ;
#13179 = CARTESIAN_POINT ( 'NONE',  ( 13.50000000000000355, 68.57999999999998408, -4.386415899144233244 ) ) ;
#13180 = CARTESIAN_POINT ( 'NONE',  ( 3.311465905292703571, 65.79890599816108931, 13.08767270555769535 ) ) ;
#13181 = CARTESIAN_POINT ( 'NONE',  ( -4.171729424061787483, 70.32999999999999829, -12.83926296998457417 ) ) ;
#13182 = CARTESIAN_POINT ( 'NONE',  ( 11.76794919243112325, 40.27999999999998693, 3.823638476888996607 ) ) ;
#13183 = CARTESIAN_POINT ( 'NONE',  ( 0.000000000000000000, 0.000000000000000000, 0.000000000000000000 ) ) ;
#13184 = CARTESIAN_POINT ( 'NONE',  ( -12.81629044767723258, 59.08368428406883766, 4.264882000424433883 ) ) ;
#13185 = CARTESIAN_POINT ( 'NONE',  ( 12.88521962934911969, 45.28541850008814151, 4.028261922845268295 ) ) ;
#13186 = CARTESIAN_POINT ( 'NONE',  ( 13.22000464319502910, 69.52673859052352157, -2.737438834081824979 ) ) ;
#13187 = CARTESIAN_POINT ( 'NONE',  ( 3.708978301276113054, 80.81333388317378308, 12.98124409862539252 ) ) ;
#13188 = CARTESIAN_POINT ( 'NONE',  ( 11.37079320667167082, 30.15738796711680081, 7.279353378998085766 ) ) ;
#13189 = CARTESIAN_POINT ( 'NONE',  ( -10.11932462375468589, 55.58550355030939727, -8.935858638386630304 ) ) ;
#13190 = CARTESIAN_POINT ( 'NONE',  ( -8.561306179327837995, 50.35156287121731822, 10.43811098430223971 ) ) ;
#13191 = CARTESIAN_POINT ( 'NONE',  ( 8.352964853697221415, 63.86126407894886370, -10.60947463986401296 ) ) ;
#13192 = CARTESIAN_POINT ( 'NONE',  ( 12.03319936400606771, 42.65557395139708063, -6.120239074458291739 ) ) ;
#13193 = CARTESIAN_POINT ( 'NONE',  ( 11.13553297422662425, 39.14273495546231629, 7.632164570861474928 ) ) ;
#13194 = ORIENTED_EDGE ( 'NONE', *, *, #1628, .T. ) ;
#13195 = CARTESIAN_POINT ( 'NONE',  ( -8.467238370142107229, 70.50394589295852654, -10.52029779368665352 ) ) ;
#13196 = CARTESIAN_POINT ( 'NONE',  ( -3.992645158735599775, 61.32355938215374636, -12.89609062310873711 ) ) ;
#13197 = CARTESIAN_POINT ( 'NONE',  ( -3.636496289402152637, 6.330000000000001847, -11.19198476289190936 ) ) ;
#13198 = ORIENTED_EDGE ( 'NONE', *, *, #3547, .T. ) ;
#13199 = ORIENTED_EDGE ( 'NONE', *, *, #9029, .F. ) ;
#13200 = CARTESIAN_POINT ( 'NONE',  ( 8.343458848123583849, 21.87999999999999545, -11.48378591275253768 ) ) ;
#13201 = CARTESIAN_POINT ( 'NONE',  ( 13.16986379959834075, -81.16874999999980389, 13.16986379960055231 ) ) ;
#13202 = CARTESIAN_POINT ( 'NONE',  ( 0.000000000000000000, 102.9300000000000068, 6.000000000000001776 ) ) ;
#13203 = CARTESIAN_POINT ( 'NONE',  ( 13.39541892358324482, 57.37148616028263604, 1.677126579065239209 ) ) ;
#13204 = APPLICATION_CONTEXT ( 'automotive_design' ) ;
#13205 = CARTESIAN_POINT ( 'NONE',  ( -3.636496289402153081, 68.32999999999999829, -11.19198476289190936 ) ) ;
#13206 = CARTESIAN_POINT ( 'NONE',  ( -3.636496289402155746, 75.53000000000000114, 11.19198476289190936 ) ) ;
#13207 = CARTESIAN_POINT ( 'NONE',  ( 4.171729424061789260, 0.8299999999999974065, 12.83926296998457239 ) ) ;
#13208 = PRESENTATION_STYLE_ASSIGNMENT (( #3572 ) ) ;
#13209 = DIRECTION ( 'NONE',  ( -1.000000000000000000, -1.301042606982605567E-16, -0.000000000000000000 ) ) ;
#13210 = CARTESIAN_POINT ( 'NONE',  ( -4.711679271994916540, -11.44687499999997371, 11.37499999999960210 ) ) ;
#13211 = LINE ( 'NONE', #8988, #2988 ) ;
#13212 = CARTESIAN_POINT ( 'NONE',  ( 5.803585914168436943, 33.96878461091537815, -12.18886560664654439 ) ) ;
#13213 = CARTESIAN_POINT ( 'NONE',  ( -4.772267704801665289, 73.35190717389953363, -12.62917378417867553 ) ) ;
#13214 = ORIENTED_EDGE ( 'NONE', *, *, #6562, .F. ) ;
#13215 = VERTEX_POINT ( 'NONE', #6763 ) ;
#13216 = CARTESIAN_POINT ( 'NONE',  ( 7.272992578804311492, 79.87999999999999545, -10.01041549318726886 ) ) ;
#13217 = VERTEX_POINT ( 'NONE', #8360 ) ;
#13218 = CARTESIAN_POINT ( 'NONE',  ( 11.37499999999960210, -72.80937499999984652, 4.711679271994916540 ) ) ;
#13219 = CARTESIAN_POINT ( 'NONE',  ( -9.654787189692980220, 44.29874787832478944, 9.440553263455338850 ) ) ;
#13220 = CARTESIAN_POINT ( 'NONE',  ( -7.499999999999994671, -23.99662210092440517, -8.932545650451688246 ) ) ;
#13221 = CARTESIAN_POINT ( 'NONE',  ( 13.34696669401933811, 66.50124740785342681, -2.033240060188988618 ) ) ;
#13222 = TOROIDAL_SURFACE ( 'NONE', #16307, 6.000000000000001776, 6.000000000000000000 ) ;
#13223 = CARTESIAN_POINT ( 'NONE',  ( 13.50000000000000355, 57.57999999999999829, -4.386415899144233244 ) ) ;
#13224 = CARTESIAN_POINT ( 'NONE',  ( -11.83441462683018308, 71.17064391044787897, 6.495893364519336188 ) ) ;
#13225 = ADVANCED_FACE ( 'NONE', ( #214 ), #12411, .T. ) ;
#13226 = CARTESIAN_POINT ( 'NONE',  ( 7.714727599200458030, -86.37187499999978968, -18.62499999999934985 ) ) ;
#13227 = CARTESIAN_POINT ( 'NONE',  ( -13.49996152797187854, 67.91463075201109234, -0.4484004657480521461 ) ) ;
#13228 = CARTESIAN_POINT ( 'NONE',  ( 18.62499999999934630, -82.20937499999980957, 7.714727599200467800 ) ) ;
#13229 = CARTESIAN_POINT ( 'NONE',  ( 3.780205736804012180E-08, 55.17999999864077409, -13.50000000000000000 ) ) ;
#13230 = VECTOR ( 'NONE', #9925, 1000.000000000000000 ) ;
#13231 = CARTESIAN_POINT ( 'NONE',  ( 11.76794919243112325, 17.42999999999999972, 1.734723475976807094E-15 ) ) ;
#13232 = DIRECTION ( 'NONE',  ( 0.000000000000000000, 1.000000000000000000, 0.000000000000000000 ) ) ;
#13233 = CARTESIAN_POINT ( 'NONE',  ( -13.46311281423534645, 64.89547304182495679, -0.9973165763568858644 ) ) ;
#13234 = CARTESIAN_POINT ( 'NONE',  ( -1.560960962377287098, 35.62388556644654614, 13.40948977943153153 ) ) ;
#13235 = CARTESIAN_POINT ( 'NONE',  ( 13.50000000000000355, 19.58000000000001606, -4.386415899144233244 ) ) ;
#13236 = ORIENTED_EDGE ( 'NONE', *, *, #8074, .T. ) ;
#13237 = CARTESIAN_POINT ( 'NONE',  ( 5.883989548015875926, 30.92926152634062475, 10.19133431864935879 ) ) ;
#13238 = CARTESIAN_POINT ( 'NONE',  ( -7.272992578804307939, 27.48000000000001108, -10.01041549318726886 ) ) ;
#13239 = CARTESIAN_POINT ( 'NONE',  ( -4.184719208025596160, 31.33046874752387012, -12.83515809457515111 ) ) ;
#13240 = FACE_OUTER_BOUND ( 'NONE', #15481, .T. ) ;
#13241 = CARTESIAN_POINT ( 'NONE',  ( 6.789432038303849559, 59.93098817131988199, 11.66862129383769897 ) ) ;
#13242 = CARTESIAN_POINT ( 'NONE',  ( -13.49999999999999822, -5.920000000000003482, 4.386415899144235908 ) ) ;
#13243 = CARTESIAN_POINT ( 'NONE',  ( -9.971704770123398731, 53.28226430956654269, 9.100406691781726565 ) ) ;
#13244 = CIRCLE ( 'NONE', #5363, 1.999999999999998224 ) ;
#13245 = CARTESIAN_POINT ( 'NONE',  ( -3.636496289402153081, 53.33000000000000540, -11.19198476289190936 ) ) ;
#13246 = CARTESIAN_POINT ( 'NONE',  ( 10.92172942406179104, 74.73000000000000398, -7.935100905948385908 ) ) ;
#13247 = EDGE_CURVE ( 'NONE', #6127, #3432, #14084, .T. ) ;
#13248 = CARTESIAN_POINT ( 'NONE',  ( 5.029058773629547119, 50.86151010740556444, 12.52835747826576451 ) ) ;
#13249 = CARTESIAN_POINT ( 'NONE',  ( -12.14893529072169009, 37.71319614887404725, -5.902479453089211070 ) ) ;
#13250 = CARTESIAN_POINT ( 'NONE',  ( 12.85437900238714093, 36.28169154084510950, 4.130910386987205918 ) ) ;
#13251 = CARTESIAN_POINT ( 'NONE',  ( -4.711679271994915652, -51.99687499999990337, 11.37499999999960210 ) ) ;
#13252 = CARTESIAN_POINT ( 'NONE',  ( -1.492738206771355713, 74.62634578251100947, 13.41930821191457568 ) ) ;
#13253 = CARTESIAN_POINT ( 'NONE',  ( -11.80473894797548873, 77.17302640020055549, 6.558943582821462392 ) ) ;
#13254 = CARTESIAN_POINT ( 'NONE',  ( -13.49997129730146028, 79.93743929743982335, 0.2167451702461970775 ) ) ;
#13255 = CARTESIAN_POINT ( 'NONE',  ( 9.520470885617715595, 14.13000000000000433, 6.917026985038135400 ) ) ;
#13256 = CARTESIAN_POINT ( 'NONE',  ( 7.499999999999999112, 106.7538932235142966, 7.532295102519074526 ) ) ;
#13257 = VERTEX_POINT ( 'NONE', #4277 ) ;
#13258 = CARTESIAN_POINT ( 'NONE',  ( 3.636496289402157078, 3.030000000000004690, -11.19198476289190936 ) ) ;
#13259 = ORIENTED_EDGE ( 'NONE', *, *, #17449, .F. ) ;
#13260 = CARTESIAN_POINT ( 'NONE',  ( -11.76794919243112325, 53.77999999999999403, -3.823638476888998827 ) ) ;
#13261 = CARTESIAN_POINT ( 'NONE',  ( -11.37500000000000000, -8.324999999999979750, -9.545674412382054647E-13 ) ) ;
#13262 = CARTESIAN_POINT ( 'NONE',  ( 7.714727599200458030, -19.77187499999995168, -18.62499999999934985 ) ) ;
#13263 = CARTESIAN_POINT ( 'NONE',  ( -8.549982208541774191E-16, -9.319999999999998508, 14.19474002721660355 ) ) ;
#13264 = CARTESIAN_POINT ( 'NONE',  ( 12.03944877831089677, 75.65508428389024687, -6.107598382801971759 ) ) ;
#13265 = CARTESIAN_POINT ( 'NONE',  ( -4.023268246324633536E-14, 69.18000000000000682, -13.50000000000000000 ) ) ;
#13266 = CARTESIAN_POINT ( 'NONE',  ( 0.4417390832689820357, 65.69588305743820911, 13.49284045995814374 ) ) ;
#13267 = CARTESIAN_POINT ( 'NONE',  ( 4.171729424061789260, 68.82999999999999829, 12.83926296998457417 ) ) ;
#13268 = CARTESIAN_POINT ( 'NONE',  ( 9.520470885617715595, 37.12999999999999545, 6.917026985038134512 ) ) ;
#13269 = EDGE_CURVE ( 'NONE', #6231, #15652, #12687, .T. ) ;
#13270 = CARTESIAN_POINT ( 'NONE',  ( -8.668252091055315134, 58.51341961490522436, -10.34967728072912685 ) ) ;
#13271 = CARTESIAN_POINT ( 'NONE',  ( 13.49636432536657793, 45.41924338305506836, 0.3133736981627452400 ) ) ;
#13272 = CARTESIAN_POINT ( 'NONE',  ( 11.94743759944812744, 69.66219602205637784, -6.285597574998869952 ) ) ;
#13273 = CARTESIAN_POINT ( 'NONE',  ( 2.445080149700053643E-15, 66.18000000000000682, -13.50000000000000000 ) ) ;
#13274 = CARTESIAN_POINT ( 'NONE',  ( 10.89794336758623139, 30.12856905013999409, 7.968289002914518804 ) ) ;
#13275 = CARTESIAN_POINT ( 'NONE',  ( -11.17210748473980253, 55.64497476832795542, -7.578533830143271643 ) ) ;
#13276 = CARTESIAN_POINT ( 'NONE',  ( -11.56639327183221866, 50.19069324002893495, 6.996189293027585521 ) ) ;
#13277 = CARTESIAN_POINT ( 'NONE',  ( 12.78700290053627597, 63.27388653237613170, 4.333656960051132323 ) ) ;
#13278 = CARTESIAN_POINT ( 'NONE',  ( 11.17787638430055530, 42.71467156718345137, -7.570014911160897420 ) ) ;
#13279 = CARTESIAN_POINT ( 'NONE',  ( 9.216665679856882676, 39.03962942028351790, 9.864241841985725401 ) ) ;
#13280 = ORIENTED_EDGE ( 'NONE', *, *, #9880, .T. ) ;
#13281 = CARTESIAN_POINT ( 'NONE',  ( -5.034154520868722393, 70.36169635399654965, -12.52728796785475041 ) ) ;
#13282 = CARTESIAN_POINT ( 'NONE',  ( -3.680674551539889983, 61.31232984300370958, -12.99219103675922504 ) ) ;
#13283 = CARTESIAN_POINT ( 'NONE',  ( -7.272992578804307939, 3.479999999999997762, -10.01041549318726886 ) ) ;
#13284 = ORIENTED_EDGE ( 'NONE', *, *, #933, .T. ) ;
#13285 = ORIENTED_EDGE ( 'NONE', *, *, #15702, .F. ) ;
#13286 = CARTESIAN_POINT ( 'NONE',  ( 10.92172942406178926, 24.13000000000001322, 7.935100905948385908 ) ) ;
#13287 = CARTESIAN_POINT ( 'NONE',  ( -1.564113515457998572E-12, -62.43749999999985079, 18.62500000000000000 ) ) ;
#13288 = CARTESIAN_POINT ( 'NONE',  ( 3.458946346613236411, 61.05562364027491640, -13.05177015192364820 ) ) ;
#13289 = CARTESIAN_POINT ( 'NONE',  ( 7.681080053067259605, 71.96880320796036301, 11.10186521252582104 ) ) ;
#13290 = CARTESIAN_POINT ( 'NONE',  ( 13.29995246372572737, 57.34789229178345948, 2.331640294117302670 ) ) ;
#13291 = CARTESIAN_POINT ( 'NONE',  ( 11.76794919243112325, 67.28000000000000114, 3.823638476888996607 ) ) ;
#13292 = CARTESIAN_POINT ( 'NONE',  ( -11.76794919243112325, 77.77999999999998693, -3.823638476888998827 ) ) ;
#13293 = CARTESIAN_POINT ( 'NONE',  ( 4.206197538246302159, 6.548267719634620398, 23.28534784291402104 ) ) ;
#13294 = CARTESIAN_POINT ( 'NONE',  ( 10.39543320068206178, -99.99999999999995737, 14.15274258188488332 ) ) ;
#13295 = DIRECTION ( 'NONE',  ( -0.000000000000000000, 1.000000000000000000, -0.000000000000000000 ) ) ;
#13296 = CARTESIAN_POINT ( 'NONE',  ( -11.37500000000039613, -26.01562499999994671, 4.711679271993002516 ) ) ;
#13297 = CARTESIAN_POINT ( 'NONE',  ( 4.489225048192535539, 34.01849207910494499, -12.73175184514909830 ) ) ;
#13298 = CARTESIAN_POINT ( 'NONE',  ( -7.517232062827917005, 73.46167874442537027, -11.21345962906566207 ) ) ;
#13299 = ORIENTED_EDGE ( 'NONE', *, *, #9339, .F. ) ;
#13300 = VERTEX_POINT ( 'NONE', #122 ) ;
#13301 = CARTESIAN_POINT ( 'NONE',  ( 11.76794919243112325, 76.28000000000000114, 3.823638476888997051 ) ) ;
#13302 = VERTEX_POINT ( 'NONE', #16281 ) ;
#13303 = CARTESIAN_POINT ( 'NONE',  ( -8.043339635996300530, -96.74374999999980673, -8.043339635997652337 ) ) ;
#13304 = ADVANCED_FACE ( 'NONE', ( #16462 ), #9864, .T. ) ;
#13305 = CARTESIAN_POINT ( 'NONE',  ( -10.12090119985971626, 44.27440800199393323, 8.934056138211790454 ) ) ;
#13306 = CARTESIAN_POINT ( 'NONE',  ( -7.499999999999992895, -26.57032277106731755, 6.479247348114219207 ) ) ;
#13307 = CARTESIAN_POINT ( 'NONE',  ( 12.79597734119763430, 66.58496463305510815, -4.302840019310315789 ) ) ;
#13308 = CARTESIAN_POINT ( 'NONE',  ( 8.343458848123578520, 41.97999999999999687, 11.48378591275254124 ) ) ;
#13309 = CARTESIAN_POINT ( 'NONE',  ( -11.83480306631655665, 71.17061613792351693, 6.495185643570378531 ) ) ;
#13310 = CARTESIAN_POINT ( 'NONE',  ( 18.62500000000064304, -84.29062499999983515, -7.714727599197335195 ) ) ;
#13311 = CARTESIAN_POINT ( 'NONE',  ( -13.42521090995868427, 67.97936017792704888, 1.419127934761323928 ) ) ;
#13312 = CARTESIAN_POINT ( 'NONE',  ( 18.62500000000000000, -26.04999999999992255, 1.560692158462880521E-12 ) ) ;
#13313 = AXIS2_PLACEMENT_3D ( 'NONE', #10478, #15838, #9331 ) ;
#13314 = DIRECTION ( 'NONE',  ( 1.000000000000000000, 8.673617379884039170E-17, -0.000000000000000000 ) ) ;
#13315 = CARTESIAN_POINT ( 'NONE',  ( -18.62500000000064659, -92.61562499999978115, 7.714727599197335195 ) ) ;
#13316 = CARTESIAN_POINT ( 'NONE',  ( -12.08625417401086466, 65.15233228621843864, 6.041222395741010054 ) ) ;
#13317 = CARTESIAN_POINT ( 'NONE',  ( -2.859817639333870343, 35.57722089168602508, 13.19986362302225658 ) ) ;
#13318 = VERTEX_POINT ( 'NONE', #3111 ) ;
#13319 = CARTESIAN_POINT ( 'NONE',  ( 19.00000000000000711, 7.773118517290098062, -1.732050807568807249 ) ) ;
#13320 = CARTESIAN_POINT ( 'NONE',  ( -2.685559703086524141, 31.27656278095842524, -13.23019760191706240 ) ) ;
#13321 = CARTESIAN_POINT ( 'NONE',  ( 0.000000000000000000, 102.9300000000000068, 0.000000000000000000 ) ) ;
#13322 = CARTESIAN_POINT ( 'NONE',  ( -3.636496289402156190, -10.47000000000000064, 11.19198476289190758 ) ) ;
#13323 = CARTESIAN_POINT ( 'NONE',  ( 6.476227018813886183, 59.91800028742412820, 11.84548389080563524 ) ) ;
#13324 = CARTESIAN_POINT ( 'NONE',  ( -4.171729424061787483, -9.669999999999998153, -12.83926296998457417 ) ) ;
#13325 = CARTESIAN_POINT ( 'NONE',  ( -4.883725581089568557, 53.50385945949214772, 12.59343935867386044 ) ) ;
#13326 = CIRCLE ( 'NONE', #11364, 12.00000000000000178 ) ;
#13327 = CARTESIAN_POINT ( 'NONE',  ( 9.520470885617715595, 52.12999999999999545, 6.917026985038134512 ) ) ;
#13328 = CARTESIAN_POINT ( 'NONE',  ( -10.92172942406178926, 69.62999999999999545, -7.935100905948389460 ) ) ;
#13329 = CARTESIAN_POINT ( 'NONE',  ( 10.82490547629966393, 51.12442037295507902, 8.066909685650703210 ) ) ;
#13330 = CARTESIAN_POINT ( 'NONE',  ( -10.26118691261005367, 37.59304863723961176, -8.772592031706285098 ) ) ;
#13331 = CARTESIAN_POINT ( 'NONE',  ( 11.71544674525831908, 36.17874677927314764, 6.766421350180369387 ) ) ;
#13332 = CARTESIAN_POINT ( 'NONE',  ( 13.16986379960055409, -9.331249999999993605, -13.16986379959834430 ) ) ;
#13333 = CARTESIAN_POINT ( 'NONE',  ( -5.282920329015465377, 74.48891104032615829, 12.42340604607010945 ) ) ;
#13334 = CARTESIAN_POINT ( 'NONE',  ( -13.29386781379963445, 76.84733676671916669, -2.350162437524830228 ) ) ;
#13335 = CIRCLE ( 'NONE', #6303, 26.00000000000000355 ) ;
#13336 = CARTESIAN_POINT ( 'NONE',  ( -13.41783933752910585, 79.86962778622965686, -1.738652325513279973 ) ) ;
#13337 = CARTESIAN_POINT ( 'NONE',  ( 7.499999999999999112, 106.0136413093990342, -8.254396200996678701 ) ) ;
#13338 = CARTESIAN_POINT ( 'NONE',  ( 3.636496289402154414, 1.829999999999998295, 11.19198476289190758 ) ) ;
#13339 = CARTESIAN_POINT ( 'NONE',  ( 9.520470885617717371, 61.72999999999999687, -6.917026985038131848 ) ) ;
#13340 = CARTESIAN_POINT ( 'NONE',  ( -11.37499999999960743, -66.63437499999983515, -4.711679271994912099 ) ) ;
#13341 = CARTESIAN_POINT ( 'NONE',  ( 18.62500000000000000, -33.29999999999991900, 1.560692158462880521E-12 ) ) ;
#13342 = CARTESIAN_POINT ( 'NONE',  ( 4.171729424061789260, -6.169999999999994600, 12.83926296998457239 ) ) ;
#13343 = ADVANCED_FACE ( 'NONE', ( #15120 ), #3018, .T. ) ;
#13344 = CARTESIAN_POINT ( 'NONE',  ( 15.58845726811991916, 7.773118517290098950, -10.99999999999996092 ) ) ;
#13345 = CARTESIAN_POINT ( 'NONE',  ( 11.73542858777253350, 75.67814331974577158, -6.690067788355273493 ) ) ;
#13346 = DIRECTION ( 'NONE',  ( -0.8660254037844343777, 0.000000000000000000, -0.5000000000000075495 ) ) ;
#13347 =( BOUNDED_CURVE ( )  B_SPLINE_CURVE ( 2, ( #1568, #2973, #2884, #7331, #12714, #601, #4500, #6987, #429, #13756, #8579, #13930, #3065 ),
 .UNSPECIFIED., .F., .F. ) 
 B_SPLINE_CURVE_WITH_KNOTS ( ( 3, 2, 2, 2, 2, 2, 3 ),
 ( 0.1673499929175705225, 0.1711054437513025994, 0.1786163454187667532, 0.1861272470862310735, 0.1936381487536952273, 0.2011490504211593811, 0.2049045012548912914 ),
 .UNSPECIFIED. ) 
 CURVE ( )  GEOMETRIC_REPRESENTATION_ITEM ( )  RATIONAL_B_SPLINE_CURVE ( ( 0.9755282581475768211, 0.9755282581475768211, 1.000000000000000000, 0.9510565162951536422, 1.000000000000000000, 0.9510565162951536422, 1.000000000000000000, 0.9510565162951536422, 1.000000000000000000, 0.9510565162951536422, 1.000000000000000000, 0.9755282581475778203, 0.9755282581475768211 ) ) 
 REPRESENTATION_ITEM ( '' )  );
#13348 = CARTESIAN_POINT ( 'NONE',  ( 7.272992578804308828, 42.97999999999998977, 10.01041549318726709 ) ) ;
#13349 = CARTESIAN_POINT ( 'NONE',  ( -7.999999999999670486, 0.000000000000000000, -24.73863375370606477 ) ) ;
#13350 = CARTESIAN_POINT ( 'NONE',  ( -12.78340117865951520, 58.77362691746088785, -4.339946196950513091 ) ) ;
#13351 = CARTESIAN_POINT ( 'NONE',  ( 3.572953084902807053, 44.80828262693227515, 13.02032272097764576 ) ) ;
#13352 = CARTESIAN_POINT ( 'NONE',  ( 13.41657896972532704, 69.37782559286166872, 1.498472742429565630 ) ) ;
#13353 = CARTESIAN_POINT ( 'NONE',  ( 0.000000000000000000, 0.000000000000000000, 0.000000000000000000 ) ) ;
#13354 = CARTESIAN_POINT ( 'NONE',  ( -12.00000000000000178, 4.063974596215564894, -2.718289652585034772E-15 ) ) ;
#13355 = CARTESIAN_POINT ( 'NONE',  ( -12.11432412061597219, 55.71088818410203203, -5.957677718900700192 ) ) ;
#13356 = CARTESIAN_POINT ( 'NONE',  ( -12.10558320543248989, 49.71015782045832765, -5.975393061918390814 ) ) ;
#13357 = CARTESIAN_POINT ( 'NONE',  ( 11.52526665190315391, 63.69236103524189474, -7.029820945411229260 ) ) ;
#13358 = CARTESIAN_POINT ( 'NONE',  ( 6.442398735761099893, 42.94338794518161961, -11.86886155631007966 ) ) ;
#13359 = CARTESIAN_POINT ( 'NONE',  ( 9.245400910555552798, 39.04103442320599271, 9.837310621197884686 ) ) ;
#13360 = ORIENTED_EDGE ( 'NONE', *, *, #1130, .F. ) ;
#13361 = CARTESIAN_POINT ( 'NONE',  ( -5.253428466288492693, 70.36999080376129712, -12.43590961766370562 ) ) ;
#13362 = CARTESIAN_POINT ( 'NONE',  ( -0.2958543223917724507, 61.19063785939420796, -13.49999999999999467 ) ) ;
#13363 = ORIENTED_EDGE ( 'NONE', *, *, #17277, .T. ) ;
#13364 = ORIENTED_EDGE ( 'NONE', *, *, #2675, .F. ) ;
#13365 = CARTESIAN_POINT ( 'NONE',  ( -13.49999999999999822, 25.78000000000000469, -4.386415899144240349 ) ) ;
#13366 = CARTESIAN_POINT ( 'NONE',  ( -12.50000000000000000, 94.93000000000002103, 1.224646799147353059E-15 ) ) ;
#13367 = CARTESIAN_POINT ( 'NONE',  ( 4.897649543255423232, 47.85658455420482937, 12.58047166699710040 ) ) ;
#13368 = CARTESIAN_POINT ( 'NONE',  ( -13.49999999999999822, 14.78000000000000647, -4.386415899144240349 ) ) ;
#13369 = CARTESIAN_POINT ( 'NONE',  ( 2.423490671691030496, 71.76716578115846801, 13.28070271859271934 ) ) ;
#13370 = CARTESIAN_POINT ( 'NONE',  ( 13.40032062549284575, 57.48717893755269870, -1.642066659324613820 ) ) ;
#13371 = CARTESIAN_POINT ( 'NONE',  ( -7.576616670048093940E-16, 69.68000000000000682, 12.37355403259654985 ) ) ;
#13372 = CARTESIAN_POINT ( 'NONE',  ( -11.76794919243112325, 78.07999999999999829, 3.823638476888994386 ) ) ;
#13373 = CARTESIAN_POINT ( 'NONE',  ( -3.903004734176718671, 47.53966149391548157, 12.92364409840641848 ) ) ;
#13374 = PRODUCT_DEFINITION_CONTEXT ( 'detailed design', #8130, 'design' ) ;
#13375 = CARTESIAN_POINT ( 'NONE',  ( -8.343458848123582072, 46.37999999999999545, 11.48378591275253768 ) ) ;
#13376 = CARTESIAN_POINT ( 'NONE',  ( 14.43775832588806196, -99.99999999999994316, 10.99793653110744174 ) ) ;
#13377 = CARTESIAN_POINT ( 'NONE',  ( 1.686577221131020821, 10.00000000000000000, -13.19627548623512325 ) ) ;
#13378 = CARTESIAN_POINT ( 'NONE',  ( -8.043339635996302306, -39.54374999999990337, -8.043339635997654113 ) ) ;
#13379 = CARTESIAN_POINT ( 'NONE',  ( 12.50000000000000000, 98.93000000000002103, 1.224646799147353059E-15 ) ) ;
#13380 = CARTESIAN_POINT ( 'NONE',  ( 11.72575753619244487, 33.67872147816529349, -6.696208405594990865 ) ) ;
#13381 = CARTESIAN_POINT ( 'NONE',  ( -9.709238084139839131, 73.56419381030619320, -9.379939381872517856 ) ) ;
#13382 = ORIENTED_EDGE ( 'NONE', *, *, #15118, .F. ) ;
#13383 = ORIENTED_EDGE ( 'NONE', *, *, #13479, .T. ) ;
#13384 = CARTESIAN_POINT ( 'NONE',  ( 9.520470885617717371, 76.73000000000000398, -6.917026985038131848 ) ) ;
#13385 = VERTEX_POINT ( 'NONE', #16808 ) ;
#13386 = ADVANCED_FACE ( 'NONE', ( #16983 ), #7547, .F. ) ;
#13387 = CARTESIAN_POINT ( 'NONE',  ( 9.538709233711902776E-13, -94.66249999999979536, -11.37499999999999645 ) ) ;
#13388 = CARTESIAN_POINT ( 'NONE',  ( -7.124923918163931447, 44.41509661022353583, 11.46745630815109429 ) ) ;
#13389 = CARTESIAN_POINT ( 'NONE',  ( 7.999999999999906741, 7.815232041205461222, 17.14738331135997740 ) ) ;
#13390 = CARTESIAN_POINT ( 'NONE',  ( 8.343458848123578520, 47.97999999999999687, 11.48378591275254124 ) ) ;
#13391 = CARTESIAN_POINT ( 'NONE',  ( -8.228354664486742465, 71.36683761322035480, 10.70256661444891222 ) ) ;
#13392 = CARTESIAN_POINT ( 'NONE',  ( -1.564113515457998370E-12, -38.53749999999988063, 18.62500000000000000 ) ) ;
#13393 = CARTESIAN_POINT ( 'NONE',  ( -13.47488564051851334, 67.95938883480165771, 0.8512204470096735864 ) ) ;
#13394 = CARTESIAN_POINT ( 'NONE',  ( -18.62499999999935341, -33.33437499999990195, -7.714727599200458030 ) ) ;
#13395 = B_SPLINE_CURVE_WITH_KNOTS ( 'NONE', 3,
 ( #16951, #1922, #4852, #10255 ),
 .UNSPECIFIED., .F., .F.,
 ( 4, 4 ),
 ( 2.376698214958262694E-07, 0.007646667280170310783 ),
 .UNSPECIFIED. ) ;
#13396 = CARTESIAN_POINT ( 'NONE',  ( 11.54421080121787391, 54.69106169426531494, -6.998656893040053006 ) ) ;
#13397 = CARTESIAN_POINT ( 'NONE',  ( -7.714727599200467800, -94.69687499999979252, 18.62499999999934630 ) ) ;
#13398 = CARTESIAN_POINT ( 'NONE',  ( -13.01035162171275772, 64.80131765794939724, -3.603924305307248055 ) ) ;
#13399 = CARTESIAN_POINT ( 'NONE',  ( -12.58169653699114043, 35.10756079940100705, 4.893995670961994726 ) ) ;
#13400 = CARTESIAN_POINT ( 'NONE',  ( -8.549982208541774191E-16, 21.68000000000000682, 14.19474002721660355 ) ) ;
#13401 = ORIENTED_EDGE ( 'NONE', *, *, #4416, .T. ) ;
#13402 = CARTESIAN_POINT ( 'NONE',  ( -5.505582777971113728, 2.022510465845309778E-14, -11.21382616413506739 ) ) ;
#13403 = LINE ( 'NONE', #2519, #13688 ) ;
#13404 = CARTESIAN_POINT ( 'NONE',  ( -2.369581839689028691, 31.26519794180775946, -13.29387509668438305 ) ) ;
#13405 = CARTESIAN_POINT ( 'NONE',  ( 11.58782070419744592, 72.68816403396648695, -6.927154233550009366 ) ) ;
#13406 = CARTESIAN_POINT ( 'NONE',  ( -10.00000000000014211, 0.000000000000000000, 17.32050807568869288 ) ) ;
#13407 = CARTESIAN_POINT ( 'NONE',  ( 4.171729424061789260, -8.169999999999996376, 12.83926296998457239 ) ) ;
#13408 = CARTESIAN_POINT ( 'NONE',  ( -2.574185747556406501, 53.58751162550813518, 13.25824297384535377 ) ) ;
#13409 = CARTESIAN_POINT ( 'NONE',  ( -9.520470885617717371, 48.23000000000000398, 6.917026985038133624 ) ) ;
#13410 = CARTESIAN_POINT ( 'NONE',  ( 13.50000000000000355, 65.57999999999998408, -4.386415899144233244 ) ) ;
#13411 = CARTESIAN_POINT ( 'NONE',  ( 10.69206503222415527, 51.11683399389762883, 8.241953851791326002 ) ) ;
#13412 = EDGE_CURVE ( 'NONE', #42, #14262, #9950, .T. ) ;
#13413 = CARTESIAN_POINT ( 'NONE',  ( -12.70032077649241131, 37.76312699646079807, -4.620871474344856900 ) ) ;
#13414 = CARTESIAN_POINT ( 'NONE',  ( 8.950850146857373346, 36.02672331505379333, 10.10926642398400332 ) ) ;
#13415 = CARTESIAN_POINT ( 'NONE',  ( -11.37499999999960210, -81.13437499999982094, -4.711679271994911211 ) ) ;
#13416 = CARTESIAN_POINT ( 'NONE',  ( -7.804728211771945645, 74.38584041582383577, 11.02015311321599889 ) ) ;
#13417 = AXIS2_PLACEMENT_3D ( 'NONE', #8910, #9977, #4743 ) ;
#13418 = CARTESIAN_POINT ( 'NONE',  ( -12.72587516454714240, 76.76713713515550808, -4.510395728399637427 ) ) ;
#13419 = CARTESIAN_POINT ( 'NONE',  ( -13.04304625457159084, 79.80563238178049801, -3.489764737285672158 ) ) ;
#13420 = CARTESIAN_POINT ( 'NONE',  ( 7.500000000000000000, 106.2113042096659257, -8.086389325435060726 ) ) ;
#13421 = CARTESIAN_POINT ( 'NONE',  ( -4.171729424061787483, 7.330000000000003624, -12.83926296998457417 ) ) ;
#13422 = CARTESIAN_POINT ( 'NONE',  ( -11.76794919243112325, 3.930000000000002824, -2.602085213965210642E-15 ) ) ;
#13423 = CARTESIAN_POINT ( 'NONE',  ( -11.76794919243112325, 50.92999999999999972, -2.882316262207890869E-15 ) ) ;
#13424 = CARTESIAN_POINT ( 'NONE',  ( -11.37499999999960387, -23.93437499999993889, -4.711679271994910323 ) ) ;
#13425 = CARTESIAN_POINT ( 'NONE',  ( -7.714727599200467800, -28.09687499999992966, 18.62499999999934630 ) ) ;
#13426 = CARTESIAN_POINT ( 'NONE',  ( 8.343458848123578520, -12.01999999999999780, 11.48378591275254124 ) ) ;
#13427 = DIRECTION ( 'NONE',  ( 0.000000000000000000, 0.000000000000000000, -1.000000000000000000 ) ) ;
#13428 = CARTESIAN_POINT ( 'NONE',  ( 6.174388639489537312, 75.95411551790840576, -12.00529625765989294 ) ) ;
#13429 = FACE_OUTER_BOUND ( 'NONE', #7058, .T. ) ;
#13430 = AXIS2_PLACEMENT_3D ( 'NONE', #13353, #4073, #16256 ) ;
#13431 = CARTESIAN_POINT ( 'NONE',  ( -9.520470885617715595, 35.62999999999999545, -6.917026985038136289 ) ) ;
#13432 = CARTESIAN_POINT ( 'NONE',  ( -9.845587001014646233, 41.28914020501957083, 9.247743145432201217 ) ) ;
#13433 = CARTESIAN_POINT ( 'NONE',  ( -5.764196172476330204, 58.38967490561365992, -12.20754040654003880 ) ) ;
#13434 = EDGE_CURVE ( 'NONE', #16561, #4303, #12585, .T. ) ;
#13435 = CARTESIAN_POINT ( 'NONE',  ( 0.000000000000000000, 9.999999999999998224, -14.50000000000000000 ) ) ;
#13436 = CARTESIAN_POINT ( 'NONE',  ( 0.000000000000000000, 80.93000000000000682, -13.50000000000000000 ) ) ;
#13437 = CYLINDRICAL_SURFACE ( 'NONE', #8752, 13.50000000000000000 ) ;
#13438 = CARTESIAN_POINT ( 'NONE',  ( -9.291548975078672612, 55.54290236572062156, -9.805807003418143708 ) ) ;
#13439 = CARTESIAN_POINT ( 'NONE',  ( -12.81046799232142419, 49.77384515584038382, -4.351227976931586916 ) ) ;
#13440 = CARTESIAN_POINT ( 'NONE',  ( 13.36172522450170241, 63.49744435280518928, -1.927315141226759732 ) ) ;
#13441 = CARTESIAN_POINT ( 'NONE',  ( 5.678863279829545974, 42.97365145709494527, -12.24748028004784572 ) ) ;
#13442 = CARTESIAN_POINT ( 'NONE',  ( 8.224463485078279845, 38.99288720330545033, 10.71476610712685051 ) ) ;
#13443 = VERTEX_POINT ( 'NONE', #7198 ) ;
#13444 = CARTESIAN_POINT ( 'NONE',  ( -9.891601304258150762, 70.57355540121815807, -9.187288538321107367 ) ) ;
#13445 = DIRECTION ( 'NONE',  ( -0.000000000000000000, 1.000000000000000000, -0.000000000000000000 ) ) ;
#13446 = VECTOR ( 'NONE', #6857, 1000.000000000000000 ) ;
#13447 = ORIENTED_EDGE ( 'NONE', *, *, #2287, .T. ) ;
#13448 = ORIENTED_EDGE ( 'NONE', *, *, #2770, .F. ) ;
#13449 = CARTESIAN_POINT ( 'NONE',  ( 2.621994543952811015E-15, 22.18000000000000327, -14.19474002721660355 ) ) ;
#13450 = CARTESIAN_POINT ( 'NONE',  ( 18.62499999999934630, -82.20937499999980957, 7.714727599200467800 ) ) ;
#13451 = CARTESIAN_POINT ( 'NONE',  ( 6.374620558230982503, 60.94607247059151689, -11.90018113148034473 ) ) ;
#13452 = CARTESIAN_POINT ( 'NONE',  ( -13.50000000000000000, 8.929999999999992610, -3.469446951953614189E-15 ) ) ;
#13453 = CARTESIAN_POINT ( 'NONE',  ( 9.378081481877091008, 72.04743592386726903, 9.715564754266829084 ) ) ;
#13454 = CARTESIAN_POINT ( 'NONE',  ( 13.50123327339441914, 57.41482836698943970, 0.4418988847496390648 ) ) ;
#13455 = CARTESIAN_POINT ( 'NONE',  ( 2.272985001014427788E-15, 71.17999999999999261, -12.37355403259654985 ) ) ;
#13456 = CARTESIAN_POINT ( 'NONE',  ( -8.343458848123582072, 34.37999999999998835, 11.48378591275254124 ) ) ;
#13457 = CARTESIAN_POINT ( 'NONE',  ( -3.636496289402153081, 74.33000000000001251, -11.19198476289190936 ) ) ;
#13458 = CARTESIAN_POINT ( 'NONE',  ( -3.140275034707463941, 47.56712421504963118, 13.13116523590432116 ) ) ;
#13459 = CARTESIAN_POINT ( 'NONE',  ( 0.000000000000000000, 75.00000000000000000, 0.000000000000000000 ) ) ;
#13460 = CARTESIAN_POINT ( 'NONE',  ( 9.708203932499419153, 8.863974596215612678, -7.053423027509713172 ) ) ;
#13461 = EDGE_CURVE ( 'NONE', #2326, #2565, #15640, .T. ) ;
#13462 = CARTESIAN_POINT ( 'NONE',  ( 6.732494237459348163, -99.99999999999981526, 15.36475110869683469 ) ) ;
#13463 = FACE_OUTER_BOUND ( 'NONE', #2048, .T. ) ;
#13464 = CARTESIAN_POINT ( 'NONE',  ( 11.37500000000000000, -16.64999999999995950, 9.531744055041752924E-13 ) ) ;
#13465 = CARTESIAN_POINT ( 'NONE',  ( 2.445080149700053643E-15, 51.18000000000000682, -13.50000000000000000 ) ) ;
#13466 = CARTESIAN_POINT ( 'NONE',  ( 13.49036936581445900, 33.44756504376105255, -0.5105335361757911139 ) ) ;
#13467 = CARTESIAN_POINT ( 'NONE',  ( -9.651347398433271607, 73.56125364406217670, -9.439358866893277522 ) ) ;
#13468 = ORIENTED_EDGE ( 'NONE', *, *, #2811, .T. ) ;
#13469 = ORIENTED_EDGE ( 'NONE', *, *, #11479, .T. ) ;
#13470 = CARTESIAN_POINT ( 'NONE',  ( -5.611269881966371109, 62.47627512215084522, 12.27858589067506934 ) ) ;
#13471 = ORIENTED_EDGE ( 'NONE', *, *, #10270, .F. ) ;
#13472 = CARTESIAN_POINT ( 'NONE',  ( -13.30519346037214135, 41.01035172162969644, 2.285875191404075579 ) ) ;
#13473 = CARTESIAN_POINT ( 'NONE',  ( -11.37499999999999645, -82.17499999999982663, -9.545674412382054647E-13 ) ) ;
#13474 = CARTESIAN_POINT ( 'NONE',  ( -0.6761224248667969672, 44.65568913397951434, 13.48306232859242293 ) ) ;
#13475 = CARTESIAN_POINT ( 'NONE',  ( -7.499999999999996447, -23.27176790847080667, -9.199276322163099096 ) ) ;
#13476 = CARTESIAN_POINT ( 'NONE',  ( 13.50000000000000000, 48.42999999999999972, 1.653273178848926867E-15 ) ) ;
#13477 = CARTESIAN_POINT ( 'NONE',  ( -10.92172942406179104, 43.22999999999999687, 7.935100905948387684 ) ) ;
#13478 = CARTESIAN_POINT ( 'NONE',  ( -12.93260499938089403, 71.06873686804253509, 3.872692500715011921 ) ) ;
#13479 = EDGE_CURVE ( 'NONE', #11794, #760, #15331, .T. ) ;
#13480 = CARTESIAN_POINT ( 'NONE',  ( -7.714727599200466912, -37.49687499999989626, 18.62499999999935341 ) ) ;
#13481 = CARTESIAN_POINT ( 'NONE',  ( -12.18806906699818882, 67.71628745454681564, -5.824626418828033891 ) ) ;
#13482 = CARTESIAN_POINT ( 'NONE',  ( -18.62500000000000000, -17.72499999999994102, -1.562973063126292757E-12 ) ) ;
#13483 = CARTESIAN_POINT ( 'NONE',  ( 11.18355001832372864, 54.71426267336678961, -7.567176262528036546 ) ) ;
#13484 = CARTESIAN_POINT ( 'NONE',  ( -9.520470885617715595, 18.63000000000000611, -6.917026985038136289 ) ) ;
#13485 = CYLINDRICAL_SURFACE ( 'NONE', #16321, 26.00000000000000355 ) ;
#13486 = CARTESIAN_POINT ( 'NONE',  ( -12.73065029274041393, 64.76630363813843871, -4.537315649280014185 ) ) ;
#13487 = CARTESIAN_POINT ( 'NONE',  ( 7.347880794884122694E-16, 0.000000000000000000, -18.00000000000000000 ) ) ;
#13488 = CARTESIAN_POINT ( 'NONE',  ( -13.34685961114456099, 35.00103985169026544, 2.027643910844264763 ) ) ;
#13489 = VERTEX_POINT ( 'NONE', #3685 ) ;
#13490 = CARTESIAN_POINT ( 'NONE',  ( -8.808033401071559965, -2.585303254002297467E-15, -9.216900067070168845 ) ) ;
#13491 = CARTESIAN_POINT ( 'NONE',  ( -10.13503849319200256, 31.58637571636829122, -8.918039105965791080 ) ) ;
#13492 = CARTESIAN_POINT ( 'NONE',  ( 6.811485724132999131, 72.92836491868227711, -11.66693257913138382 ) ) ;
#13493 = CARTESIAN_POINT ( 'NONE',  ( -7.409984580736203970E-16, -13.32000000000000028, 12.37355403259654985 ) ) ;
#13494 = CARTESIAN_POINT ( 'NONE',  ( 0.000000000000000000, 9.000000000000000000, 0.000000000000000000 ) ) ;
#13495 = CARTESIAN_POINT ( 'NONE',  ( -13.47895445410198612, 52.90400025295915043, -0.7535177491850849618 ) ) ;
#13496 = CARTESIAN_POINT ( 'NONE',  ( -11.76794919243112325, 47.77999999999999403, -3.823638476888998827 ) ) ;
#13497 = CARTESIAN_POINT ( 'NONE',  ( 10.92172942406179104, 68.73000000000000398, -7.935100905948385908 ) ) ;
#13498 = CARTESIAN_POINT ( 'NONE',  ( 10.61679899383538483, 51.11259005245373999, 8.339111544401394127 ) ) ;
#13499 = AXIS2_PLACEMENT_3D ( 'NONE', #15597, #9001, #6010 ) ;
#13500 = CARTESIAN_POINT ( 'NONE',  ( -5.616158569158017144, 37.38391327537662789, -12.27641445107196105 ) ) ;
#13501 = CARTESIAN_POINT ( 'NONE',  ( 7.311491871512308727, 35.95290065796121581, 11.35084104978724895 ) ) ;
#13502 = CARTESIAN_POINT ( 'NONE',  ( -7.714727599197334307, -12.45312499999998757, -18.62500000000064659 ) ) ;
#13503 = CARTESIAN_POINT ( 'NONE',  ( -11.68704921467410784, 74.18220605320536265, 6.786032449176635062 ) ) ;
#13504 = CARTESIAN_POINT ( 'NONE',  ( -11.20590004775074355, 76.64706285525832641, -7.528468286527173703 ) ) ;
#13505 = CARTESIAN_POINT ( 'NONE',  ( -10.71293590878329205, 79.61766727756590001, -8.226627743301476059 ) ) ;
#13506 = CARTESIAN_POINT ( 'NONE',  ( -7.321446643557331768, 80.92999999999996419, 10.20755442051737205 ) ) ;
#13507 = CARTESIAN_POINT ( 'NONE',  ( 9.520470885617717371, 5.730000000000012861, -6.917026985038131848 ) ) ;
#13508 = CARTESIAN_POINT ( 'NONE',  ( -11.76794919243112325, 44.92999999999999972, -2.882316262207890869E-15 ) ) ;
#13509 = CARTESIAN_POINT ( 'NONE',  ( -11.37500000000039613, -26.01562499999994671, 4.711679271993002516 ) ) ;
#13510 = CARTESIAN_POINT ( 'NONE',  ( 18.62500000000064304, -1.040624999999997469, -7.714727599197335195 ) ) ;
#13511 = CARTESIAN_POINT ( 'NONE',  ( 10.92172942406179104, -8.269999999999999574, -7.935100905948385908 ) ) ;
#13512 = CARTESIAN_POINT ( 'NONE',  ( -5.995934488988542199, 40.39877640253387625, -12.09682232891648468 ) ) ;
#13513 = PLANE ( 'NONE',  #7441 ) ;
#13514 = CARTESIAN_POINT ( 'NONE',  ( 10.27758411003093819, 75.09396747692687768, 8.753359694643265243 ) ) ;
#13515 = EDGE_CURVE ( 'NONE', #760, #13131, #6948, .T. ) ;
#13516 = CARTESIAN_POINT ( 'NONE',  ( 3.922300570379358309, 5.783373742538366110E-16, -15.41399705783805807 ) ) ;
#13517 = CARTESIAN_POINT ( 'NONE',  ( 2.272985001014427788E-15, 38.17999999999999972, -12.37355403259654985 ) ) ;
#13518 = CARTESIAN_POINT ( 'NONE',  ( -11.57650647816374700, 41.18894672448205796, 6.947845214036406425 ) ) ;
#13519 = CARTESIAN_POINT ( 'NONE',  ( -11.17817305665808014, 58.64534897024895344, -7.569578125800211055 ) ) ;
#13520 = CARTESIAN_POINT ( 'NONE',  ( 2.914010673256763440, 44.78477707381765782, 13.18175074847055761 ) ) ;
#13521 = CARTESIAN_POINT ( 'NONE',  ( 4.171729424061789260, 58.82999999999999829, 12.83926296998457417 ) ) ;
#13522 = CARTESIAN_POINT ( 'NONE',  ( 7.392150717925613179, 29.95598776866237145, 11.32059538698433165 ) ) ;
#13523 = AXIS2_PLACEMENT_3D ( 'NONE', #14457, #6356, #11487 ) ;
#13524 = CARTESIAN_POINT ( 'NONE',  ( 10.00000000000002132, 0.000000000000000000, -15.32050807568876394 ) ) ;
#13525 = CARTESIAN_POINT ( 'NONE',  ( -12.11427638989693101, 49.71086542188117363, -5.957774775766911723 ) ) ;
#13526 = CARTESIAN_POINT ( 'NONE',  ( 13.47352731021837258, 63.40080362853115048, 0.8451059437790031659 ) ) ;
#13527 = CARTESIAN_POINT ( 'NONE',  ( 13.48004015203407668, 42.40468154064383555, 0.7338770590801271254 ) ) ;
#13528 = CARTESIAN_POINT ( 'NONE',  ( -18.18340077413956735, 8.007813497946154158, -0.8546369493910546122 ) ) ;
#13529 = ORIENTED_EDGE ( 'NONE', *, *, #8549, .F. ) ;
#13530 = CARTESIAN_POINT ( 'NONE',  ( -3.708203932499370303, 4.396025403784443952, 11.41267819554184371 ) ) ;
#13531 = CARTESIAN_POINT ( 'NONE',  ( -13.49999999999999822, 49.07999999999999829, 4.386415899144235020 ) ) ;
#13532 = CARTESIAN_POINT ( 'NONE',  ( -8.549982208541774191E-16, 11.67999999999999972, 14.19474002721660355 ) ) ;
#13533 = ORIENTED_EDGE ( 'NONE', *, *, #5543, .F. ) ;
#13534 = CARTESIAN_POINT ( 'NONE',  ( -5.576931461581311034, 43.38239337497184067, -12.29436833682542307 ) ) ;
#13535 = CARTESIAN_POINT ( 'NONE',  ( -7.499999999999998224, 104.2017679084707851, 9.199276322163095543 ) ) ;
#13536 = EDGE_CURVE ( 'NONE', #13571, #7996, #12690, .T. ) ;
#13537 = CARTESIAN_POINT ( 'NONE',  ( 11.86384666090724416, 60.66867754764784593, -6.447385887097871304 ) ) ;
#13538 = CARTESIAN_POINT ( 'NONE',  ( 8.343458848123583849, 10.88000000000001322, -11.48378591275253768 ) ) ;
#13539 = CARTESIAN_POINT ( 'NONE',  ( -8.891200544363830713E-16, 7.546025403784439867, 12.00000000000000000 ) ) ;
#13540 = CARTESIAN_POINT ( 'NONE',  ( 7.779282341488525709, 56.97302794364081535, 11.03737104057997165 ) ) ;
#13541 = CARTESIAN_POINT ( 'NONE',  ( -11.76794919243112325, 65.93000000000000682, -2.882316262207890869E-15 ) ) ;
#13542 = CARTESIAN_POINT ( 'NONE',  ( 11.76794919243112325, 67.28000000000000114, 3.823638476888996607 ) ) ;
#13543 = CARTESIAN_POINT ( 'NONE',  ( -4.473130523687919968, 47.51903911116670542, 12.74611812840811176 ) ) ;
#13544 = CARTESIAN_POINT ( 'NONE',  ( 5.281167590608333740, 45.98876608056069415, -12.42463402102491621 ) ) ;
#13545 = CARTESIAN_POINT ( 'NONE',  ( 0.8552964561739553329, 8.007719221390678044, -18.18372103750114022 ) ) ;
#13546 = CARTESIAN_POINT ( 'NONE',  ( 3.593849725469707490, -100.0000000000000711, 14.39518146399953480 ) ) ;
#13547 = CARTESIAN_POINT ( 'NONE',  ( -0.8894075400429002354, 56.64828133586323133, 13.47800860622838393 ) ) ;
#13548 = CARTESIAN_POINT ( 'NONE',  ( -9.552639591052204498E-13, -62.43749999999985079, 11.37500000000000000 ) ) ;
#13549 = CARTESIAN_POINT ( 'NONE',  ( 8.378362625313673817, -1.749711886770878784E-15, 10.58551083881864407 ) ) ;
#13550 = AXIS2_PLACEMENT_3D ( 'NONE', #2181, #4948, #12901 ) ;
#13551 = CARTESIAN_POINT ( 'NONE',  ( 13.48726538980810474, 33.45020437573430172, -0.5866928101883699398 ) ) ;
#13552 = CARTESIAN_POINT ( 'NONE',  ( -3.847640698436238349, 73.31827516608075257, -12.94019317380912959 ) ) ;
#13553 = DIRECTION ( 'NONE',  ( 0.000000000000000000, 0.000000000000000000, -1.000000000000000000 ) ) ;
#13554 = VERTEX_POINT ( 'NONE', #832 ) ;
#13555 = CARTESIAN_POINT ( 'NONE',  ( -3.922215051620934645, 62.53897161928807691, 12.91767269693318276 ) ) ;
#13556 =( BOUNDED_CURVE ( )  B_SPLINE_CURVE ( 2, ( #1706, #4634, #7468, #3386, #1791, #15390, #16643, #13892, #8885, #5886, #12588, #15302, #16902 ),
 .UNSPECIFIED., .F., .F. ) 
 B_SPLINE_CURVE_WITH_KNOTS ( ( 3, 2, 2, 2, 2, 2, 3 ),
 ( 0.5694444444444444198, 0.5722222222222221877, 0.5777777777777777235, 0.5833333333333333703, 0.5888888888888889062, 0.5944444444444444420, 0.5972222222222222099 ),
 .UNSPECIFIED. ) 
 CURVE ( )  GEOMETRIC_REPRESENTATION_ITEM ( )  RATIONAL_B_SPLINE_CURVE ( ( 0.9755282581475768211, 0.9755282581475768211, 1.000000000000000000, 0.9510565162951535312, 1.000000000000000000, 0.9510565162951535312, 1.000000000000000000, 0.9510565162951535312, 1.000000000000000000, 0.9510565162951535312, 1.000000000000000000, 0.9755282581475768211, 0.9755282581475768211 ) ) 
 REPRESENTATION_ITEM ( '' )  );
#13557 = ORIENTED_EDGE ( 'NONE', *, *, #8002, .F. ) ;
#13558 = CARTESIAN_POINT ( 'NONE',  ( 3.636496289402154414, -16.16999999999999815, 11.19198476289190758 ) ) ;
#13559 = CARTESIAN_POINT ( 'NONE',  ( 11.37499999999999645, -90.49999999999980105, 9.531744055041752924E-13 ) ) ;
#13560 = CARTESIAN_POINT ( 'NONE',  ( -13.10259906904691896, 44.04626536728174102, 3.264601644182080875 ) ) ;
#13561 = ADVANCED_FACE ( 'NONE', ( #3488 ), #7305, .F. ) ;
#13562 = CARTESIAN_POINT ( 'NONE',  ( -7.499999999999992895, -27.79580463407382851, -1.043242051446495733 ) ) ;
#13563 = CARTESIAN_POINT ( 'NONE',  ( 2.607531440858944223E-15, 43.17999999999999972, -14.19474002721660355 ) ) ;
#13564 = CARTESIAN_POINT ( 'NONE',  ( -13.47393936470618137, 70.95918448809980816, 0.8439462952680778507 ) ) ;
#13565 = CARTESIAN_POINT ( 'NONE',  ( 13.16986379960055409, -44.78124999999987921, -13.16986379959834430 ) ) ;
#13566 = CARTESIAN_POINT ( 'NONE',  ( -13.42870403230521958, 67.88181673837877383, -1.385841348755903590 ) ) ;
#13567 = CARTESIAN_POINT ( 'NONE',  ( 7.714727599197338748, -96.77812499999976126, 18.62500000000063949 ) ) ;
#13568 = CARTESIAN_POINT ( 'NONE',  ( 11.54108203963314239, 54.69126936105765679, -7.003815892991897663 ) ) ;
#13569 = FACE_OUTER_BOUND ( 'NONE', #15101, .T. ) ;
#13570 = CARTESIAN_POINT ( 'NONE',  ( -12.71393839463805797, 65.09396562736293390, 4.539402788875312567 ) ) ;
#13571 = VERTEX_POINT ( 'NONE', #10140 ) ;
#13572 = CARTESIAN_POINT ( 'NONE',  ( -4.171729424061787483, 63.32999999999999829, -12.83926296998457417 ) ) ;
#13573 = CARTESIAN_POINT ( 'NONE',  ( -13.46032330647282826, 34.89419764945687774, -1.036509372401692053 ) ) ;
#13574 = ORIENTED_EDGE ( 'NONE', *, *, #13148, .T. ) ;
#13575 = CARTESIAN_POINT ( 'NONE',  ( 13.39701859097131909, 78.37195839092206029, 1.664708910713033507 ) ) ;
#13576 = CARTESIAN_POINT ( 'NONE',  ( -12.44161054033546776, 4.250271015223983793E-15, -4.165684030147709827 ) ) ;
#13577 = CARTESIAN_POINT ( 'NONE',  ( -11.52056222259168372, 31.66712582499730999, -7.043476334750435441 ) ) ;
#13578 = CARTESIAN_POINT ( 'NONE',  ( 10.16376560654192218, 72.77214537080571688, -8.885750376373021453 ) ) ;
#13579 = CARTESIAN_POINT ( 'NONE',  ( -7.272992578804310604, -13.62000000000000632, 10.01041549318726709 ) ) ;
#13580 = DIRECTION ( 'NONE',  ( 0.000000000000000000, 0.000000000000000000, 1.000000000000000000 ) ) ;
#13581 = CARTESIAN_POINT ( 'NONE',  ( -13.49999999999999822, -17.92000000000000526, 4.386415899144235908 ) ) ;
#13582 = CARTESIAN_POINT ( 'NONE',  ( -4.171729424061787483, 73.33000000000001251, -12.83926296998457417 ) ) ;
#13583 = CARTESIAN_POINT ( 'NONE',  ( -12.86141184943314109, 52.78247262265329454, -4.106605482048742317 ) ) ;
#13584 = CARTESIAN_POINT ( 'NONE',  ( 11.76794919243112325, 46.42999999999999972, 1.441158131103945434E-15 ) ) ;
#13585 = CARTESIAN_POINT ( 'NONE',  ( 2.607531440858944223E-15, 63.17999999999999972, -14.19474002721660355 ) ) ;
#13586 = AXIS2_PLACEMENT_3D ( 'NONE', #5031, #10515, #5300 ) ;
#13587 = CARTESIAN_POINT ( 'NONE',  ( 8.069076079402949020, 50.98598018282910971, 10.82319128239823236 ) ) ;
#13588 = CARTESIAN_POINT ( 'NONE',  ( -4.930242145783458874, 37.35776634295052645, -12.56953676492723204 ) ) ;
#13589 = CARTESIAN_POINT ( 'NONE',  ( 10.66331449835562140, 36.11497312102070367, 8.282658568296689339 ) ) ;
#13590 = CARTESIAN_POINT ( 'NONE',  ( 11.37499999999999645, -90.49999999999980105, 9.531744055041752924E-13 ) ) ;
#13591 = CARTESIAN_POINT ( 'NONE',  ( -11.99159045330921813, 74.15881072468002344, 6.200948343019899944 ) ) ;
#13592 = CARTESIAN_POINT ( 'NONE',  ( -13.49332011507778617, 76.94460881575584210, 0.4250470828855623662 ) ) ;
#13593 = CARTESIAN_POINT ( 'NONE',  ( -5.572961361443443451, 79.38198842499259911, -12.30395537494314695 ) ) ;
#13594 = DIRECTION ( 'NONE',  ( 0.000000000000000000, -0.000000000000000000, 1.000000000000000000 ) ) ;
#13595 = CARTESIAN_POINT ( 'NONE',  ( 0.2248552520803865362, 80.93000000000003524, 13.08843060417372151 ) ) ;
#13596 = CARTESIAN_POINT ( 'NONE',  ( -3.636496289402152637, 0.3299999999999969624, -11.19198476289190936 ) ) ;
#13597 = CARTESIAN_POINT ( 'NONE',  ( 11.76794919243112325, 43.42999999999999972, 1.441158131103945434E-15 ) ) ;
#13598 = CARTESIAN_POINT ( 'NONE',  ( 7.714727599200458030, -3.121874999999992628, -18.62499999999934985 ) ) ;
#13599 = CARTESIAN_POINT ( 'NONE',  ( -4.171729424061787483, -16.66999999999999815, -12.83926296998457417 ) ) ;
#13600 = VECTOR ( 'NONE', #13632, 1000.000000000000000 ) ;
#13601 = CARTESIAN_POINT ( 'NONE',  ( -19.00000000000001776, 0.000000000000000000, 1.732050807568674466 ) ) ;
#13602 = CARTESIAN_POINT ( 'NONE',  ( 11.47620768244502898, 75.16437255002460915, 7.109921825326903644 ) ) ;
#13603 = CARTESIAN_POINT ( 'NONE',  ( 8.417131036019558366, -3.230386817174870386E-14, -15.11476970363428407 ) ) ;
#13604 = CARTESIAN_POINT ( 'NONE',  ( -7.272992578804307939, 32.47999999999999687, -10.01041549318726886 ) ) ;
#13605 = CARTESIAN_POINT ( 'NONE',  ( -9.286236634453807426, 41.31697598119224324, 9.798817830080201574 ) ) ;
#13606 = CARTESIAN_POINT ( 'NONE',  ( -12.76045986475135585, 58.77107810914377239, -4.407033307690351620 ) ) ;
#13607 = CARTESIAN_POINT ( 'NONE',  ( 4.654608482077335019, 44.84757688545764154, 12.67221841744786559 ) ) ;
#13608 = VECTOR ( 'NONE', #11590, 1000.000000000000000 ) ;
#13609 = CARTESIAN_POINT ( 'NONE',  ( -8.891200544363830713E-16, 55.67999999999999972, 13.50000000000000000 ) ) ;
#13610 = DIRECTION ( 'NONE',  ( 0.000000000000000000, 0.000000000000000000, 1.000000000000000000 ) ) ;
#13611 = EDGE_CURVE ( 'NONE', #11272, #7647, #4022, .T. ) ;
#13612 = FACE_OUTER_BOUND ( 'NONE', #13870, .T. ) ;
#13613 = CARTESIAN_POINT ( 'NONE',  ( -9.404872160078671328, 49.54852003193013132, -9.698209604899176384 ) ) ;
#13614 = CARTESIAN_POINT ( 'NONE',  ( 10.28911076424348892, 63.76544862978350636, -8.742538089261900680 ) ) ;
#13615 = CARTESIAN_POINT ( 'NONE',  ( 13.34880532577127177, 42.50252970743873249, -2.070817942779479282 ) ) ;
#13616 = CARTESIAN_POINT ( 'NONE',  ( 3.534134406043794474, 49.05403510232272879, -13.14852249132305140 ) ) ;
#13617 = ORIENTED_EDGE ( 'NONE', *, *, #10473, .T. ) ;
#13618 = CARTESIAN_POINT ( 'NONE',  ( 2.222800136090958073E-15, 3.046025403784441643, -12.00000000000000000 ) ) ;
#13619 = FACE_OUTER_BOUND ( 'NONE', #6249, .T. ) ;
#13620 = EDGE_LOOP ( 'NONE', ( #13214, #15853, #3317, #8170 ) ) ;
#13621 = CARTESIAN_POINT ( 'NONE',  ( -3.959965371964460079, 43.32238572718495107, -12.90617264008083076 ) ) ;
#13622 = CARTESIAN_POINT ( 'NONE',  ( -7.500000000000001776, 103.1885367479068947, -9.367496997597607233 ) ) ;
#13623 = CARTESIAN_POINT ( 'NONE',  ( 11.54232513752469202, 60.69116484201946804, -7.001836541325773489 ) ) ;
#13624 = CARTESIAN_POINT ( 'NONE',  ( -13.49999999999999822, 8.780000000000004690, -4.386415899144240349 ) ) ;
#13625 = CIRCLE ( 'NONE', #6031, 1.999999999999998224 ) ;
#13626 = CARTESIAN_POINT ( 'NONE',  ( -12.00000000000000178, 6.646025403784432406, -3.899036354794879422 ) ) ;
#13627 = CARTESIAN_POINT ( 'NONE',  ( 13.47309748709204769, 66.46350195002293049, -0.9713120919723320368 ) ) ;
#13628 = CARTESIAN_POINT ( 'NONE',  ( 3.015054115773358134, 56.78848833989679434, 13.15920921728376491 ) ) ;
#13629 = CARTESIAN_POINT ( 'NONE',  ( 3.636496289402157078, 59.03000000000000114, -11.19198476289190936 ) ) ;
#13630 = CARTESIAN_POINT ( 'NONE',  ( 7.272992578804308828, 69.97999999999998977, 10.01041549318726709 ) ) ;
#13631 = CARTESIAN_POINT ( 'NONE',  ( -11.89520195798273328, 47.16632926303795159, 6.387517813708311287 ) ) ;
#13632 = DIRECTION ( 'NONE',  ( -0.000000000000000000, -1.000000000000000000, -0.000000000000000000 ) ) ;
#13633 = CARTESIAN_POINT ( 'NONE',  ( 17.69225355208303085, -100.0000000000000000, 5.474315037022701169 ) ) ;
#13634 = EDGE_CURVE ( 'NONE', #17255, #8460, #3403, .T. ) ;
#13635 = CARTESIAN_POINT ( 'NONE',  ( -2.021337026714439489, 56.60737098508230503, 13.34784511190158440 ) ) ;
#13636 = CARTESIAN_POINT ( 'NONE',  ( 11.37499999999960210, -65.55937499999984652, 4.711679271994918317 ) ) ;
#13637 = CARTESIAN_POINT ( 'NONE',  ( 8.343458848123580296, 5.980000000000005755, 11.48378591275253768 ) ) ;
#13638 = CARTESIAN_POINT ( 'NONE',  ( 10.97843994255461908, 33.72687523005959065, -7.868560920089366029 ) ) ;
#13639 = DIRECTION ( 'NONE',  ( -0.000000000000000000, 1.000000000000000000, -0.000000000000000000 ) ) ;
#13640 = CARTESIAN_POINT ( 'NONE',  ( -9.738246541212287610, 8.018245899431759582, -15.33333167467629821 ) ) ;
#13641 = ORIENTED_EDGE ( 'NONE', *, *, #15079, .T. ) ;
#13642 = CARTESIAN_POINT ( 'NONE',  ( -2.117782281948723977, 62.60385290822299709, 13.33293114825980297 ) ) ;
#13643 = VERTEX_POINT ( 'NONE', #7661 ) ;
#13644 = CARTESIAN_POINT ( 'NONE',  ( -13.16986379960055409, -17.65624999999997513, 13.16986379959834252 ) ) ;
#13645 = CARTESIAN_POINT ( 'NONE',  ( -13.47586914819473414, 43.90198424617900486, -0.8086415342413884044 ) ) ;
#13646 = CARTESIAN_POINT ( 'NONE',  ( 13.50000000000000355, 0.5800000000000020695, -4.386415899144233244 ) ) ;
#13647 = CARTESIAN_POINT ( 'NONE',  ( 8.343458848123583849, 45.87999999999999545, -11.48378591275253768 ) ) ;
#13648 = CARTESIAN_POINT ( 'NONE',  ( -13.46831384632932327, 70.96207412421891547, 0.9270688974616148048 ) ) ;
#13649 = CARTESIAN_POINT ( 'NONE',  ( -13.16986379960055409, -69.75624999999980957, 13.16986379959834252 ) ) ;
#13650 = EDGE_CURVE ( 'NONE', #2674, #7575, #578, .T. ) ;
#13651 = CARTESIAN_POINT ( 'NONE',  ( -4.340783059308429337, 67.33576598374806110, -12.79059142491898449 ) ) ;
#13652 = CARTESIAN_POINT ( 'NONE',  ( 1.561832610794586740E-12, -80.16249999999979536, -18.62500000000000000 ) ) ;
#13653 = CARTESIAN_POINT ( 'NONE',  ( 12.99037541014949504, 54.56130944003646022, -3.674264842619463067 ) ) ;
#13654 = CARTESIAN_POINT ( 'NONE',  ( -0.4240723324158873764, 64.19524804890893677, -13.49336454334395086 ) ) ;
#13655 = VERTEX_POINT ( 'NONE', #754 ) ;
#13656 = CARTESIAN_POINT ( 'NONE',  ( 15.34527529650332411, 7.924527530346058057, -10.35822530491750371 ) ) ;
#13657 = CARTESIAN_POINT ( 'NONE',  ( -12.71024981273410681, 34.76417616951957257, -4.593182735545670248 ) ) ;
#13658 = ORIENTED_EDGE ( 'NONE', *, *, #1177, .F. ) ;
#13659 = CARTESIAN_POINT ( 'NONE',  ( 13.47158690398116043, 78.46026125564927156, -0.8756916466218195305 ) ) ;
#13660 = CARTESIAN_POINT ( 'NONE',  ( -1.271258255638932022, -3.026718717157247666E-15, -12.11055032353875305 ) ) ;
#13661 = DIRECTION ( 'NONE',  ( 0.000000000000000000, 0.000000000000000000, -1.000000000000000000 ) ) ;
#13662 = CARTESIAN_POINT ( 'NONE',  ( 10.80751904294156240, 72.73667749500260982, -8.095150784743120553 ) ) ;
#13663 = CARTESIAN_POINT ( 'NONE',  ( 4.690695874063101733, 59.84888257105829723, 12.65971414261017536 ) ) ;
#13664 = CARTESIAN_POINT ( 'NONE',  ( 10.92172942406178926, -13.87000000000000099, 7.935100905948385908 ) ) ;
#13665 = CARTESIAN_POINT ( 'NONE',  ( -8.691771469529815392E-16, 68.68000000000000682, 14.19474002721660355 ) ) ;
#13666 = CARTESIAN_POINT ( 'NONE',  ( -11.27793812523095696, 52.65156426295828140, -7.420298747894694458 ) ) ;
#13667 = CARTESIAN_POINT ( 'NONE',  ( 11.76794919243112325, 49.28000000000000114, 3.823638476888996607 ) ) ;
#13668 = CARTESIAN_POINT ( 'NONE',  ( 10.92172942406179104, 62.73000000000001108, -7.935100905948385908 ) ) ;
#13669 = CARTESIAN_POINT ( 'NONE',  ( -16.17792858571901959, 8.007293667506184320, -8.349340579021800934 ) ) ;
#13670 = CARTESIAN_POINT ( 'NONE',  ( 11.64809207761678600, 69.17605374645687277, 6.824371320973884103 ) ) ;
#13671 = LINE ( 'NONE', #1824, #16038 ) ;
#13672 = EDGE_CURVE ( 'NONE', #9583, #5339, #4912, .T. ) ;
#13673 = CARTESIAN_POINT ( 'NONE',  ( -9.552639591052204498E-13, -102.9874999999997698, 11.37499999999999645 ) ) ;
#13674 = CARTESIAN_POINT ( 'NONE',  ( -13.02432634260977018, 74.05675360358792148, 3.552071022051288551 ) ) ;
#13675 = CARTESIAN_POINT ( 'NONE',  ( -13.48935192615955359, 76.94856188004330022, 0.5393466570965053108 ) ) ;
#13676 = CARTESIAN_POINT ( 'NONE',  ( -1.732050807568877859, 7.773118517290099838, -18.99999999999999645 ) ) ;
#13677 = PLANE ( 'NONE',  #5260 ) ;
#13678 = CARTESIAN_POINT ( 'NONE',  ( -1.003751346110120011E-07, 3.679997203684337137, 13.49999999999999822 ) ) ;
#13679 = CARTESIAN_POINT ( 'NONE',  ( -13.50000000000000000, 32.93000000000001393, -3.469446951953614189E-15 ) ) ;
#13680 = CARTESIAN_POINT ( 'NONE',  ( 2.279995255611139653E-15, -8.820000000000000284, -12.37355403259654985 ) ) ;
#13681 = CARTESIAN_POINT ( 'NONE',  ( 3.636496289402157078, 44.03000000000000114, -11.19198476289190936 ) ) ;
#13682 = CARTESIAN_POINT ( 'NONE',  ( -2.138189944381240881, 2.603118577679737644, 13.49999999999999822 ) ) ;
#13683 = CARTESIAN_POINT ( 'NONE',  ( -2.005948350121168566, 34.25209037325986827, -13.35772390745884231 ) ) ;
#13684 = CARTESIAN_POINT ( 'NONE',  ( 13.30271350194304425, 75.34913341900526973, 2.300714643417195671 ) ) ;
#13685 = CARTESIAN_POINT ( 'NONE',  ( 3.612098337086700806, 8.305967389344668621E-17, -15.28315401015443165 ) ) ;
#13686 = CARTESIAN_POINT ( 'NONE',  ( -4.038158833338649778, 41.53487022600332779, 12.88215458262367186 ) ) ;
#13687 = CARTESIAN_POINT ( 'NONE',  ( -2.368957647454752458, 58.26517897696810167, -13.29052651228837334 ) ) ;
#13688 = VECTOR ( 'NONE', #14545, 1000.000000000000000 ) ;
#13689 = CARTESIAN_POINT ( 'NONE',  ( 2.044753778131714217, 44.75340735468392239, 13.35174435036512364 ) ) ;
#13690 = EDGE_CURVE ( 'NONE', #9213, #14960, #12777, .T. ) ;
#13691 = CARTESIAN_POINT ( 'NONE',  ( -10.92172942406179104, 55.23000000000000398, 7.935100905948387684 ) ) ;
#13692 = CARTESIAN_POINT ( 'NONE',  ( -10.92172942406178926, 4.629999999999995453, -7.935100905948389460 ) ) ;
#13693 = CARTESIAN_POINT ( 'NONE',  ( -9.708203932499392508, 1.363974596215586033, 7.053423027509694521 ) ) ;
#13694 = CARTESIAN_POINT ( 'NONE',  ( -11.98418087806660637, 49.70050671477787319, -6.216030342912470807 ) ) ;
#13695 = CARTESIAN_POINT ( 'NONE',  ( 11.56350959312967852, 63.17024669828877137, 6.966726136713456086 ) ) ;
#13696 = CARTESIAN_POINT ( 'NONE',  ( 8.520149165853723616, 42.00650817108029145, 10.47262060954012597 ) ) ;
#13697 = CARTESIAN_POINT ( 'NONE',  ( -18.85006967243203491, 7.815232008520037077, -1.645488492588025098 ) ) ;
#13698 = EDGE_LOOP ( 'NONE', ( #745, #16733 ) ) ;
#13699 = CARTESIAN_POINT ( 'NONE',  ( -7.576616670048093940E-16, 72.67999999999999261, 12.37355403259654807 ) ) ;
#13700 = DIRECTION ( 'NONE',  ( -0.8660254037844382635, 0.000000000000000000, 0.5000000000000008882 ) ) ;
#13701 = CARTESIAN_POINT ( 'NONE',  ( 11.37500000000000000, -16.64999999999995950, 9.531744055041752924E-13 ) ) ;
#13702 = CARTESIAN_POINT ( 'NONE',  ( -8.343458848123582072, 8.380000000000002558, 11.48378591275254124 ) ) ;
#13703 = VERTEX_POINT ( 'NONE', #14257 ) ;
#13704 = CARTESIAN_POINT ( 'NONE',  ( -2.545557221017204608, 43.27152815613324321, -13.25833315176517146 ) ) ;
#13705 = DIRECTION ( 'NONE',  ( 0.000000000000000000, -1.000000000000000000, 0.000000000000000000 ) ) ;
#13706 = CARTESIAN_POINT ( 'NONE',  ( 11.57090963045782495, 60.68925666067695346, -6.954428157688981038 ) ) ;
#13707 = CIRCLE ( 'NONE', #6116, 26.00000000000000355 ) ;
#13708 = CARTESIAN_POINT ( 'NONE',  ( 8.343458848123578520, 6.980000000000003979, 11.48378591275254124 ) ) ;
#13709 = DIRECTION ( 'NONE',  ( -0.000000000000000000, -1.000000000000000000, -0.000000000000000000 ) ) ;
#13710 = CARTESIAN_POINT ( 'NONE',  ( 9.921642846735080568, 66.78487043750489249, -9.154839053872199983 ) ) ;
#13711 = CARTESIAN_POINT ( 'NONE',  ( 1.898648508014808112, 56.74827747273968725, 13.36670787604589705 ) ) ;
#13712 = CARTESIAN_POINT ( 'NONE',  ( 11.76794919243112680, 61.57999999999999829, -3.823638476888993942 ) ) ;
#13713 = CARTESIAN_POINT ( 'NONE',  ( 4.171729424061791924, 36.03000000000000114, -12.83926296998457239 ) ) ;
#13714 = CARTESIAN_POINT ( 'NONE',  ( -11.76794919243112325, 62.92999999999999972, -2.882316262207890869E-15 ) ) ;
#13715 = CARTESIAN_POINT ( 'NONE',  ( -13.49555206794069306, 46.94222366541166025, 0.3561146266941883631 ) ) ;
#13716 = DIRECTION ( 'NONE',  ( 0.000000000000000000, 1.000000000000000000, 0.000000000000000000 ) ) ;
#13717 = CARTESIAN_POINT ( 'NONE',  ( 1.645540471734042054, 7.815206720109964422, -18.85015970295421894 ) ) ;
#13718 = CARTESIAN_POINT ( 'NONE',  ( 10.07123223633273490, 30.77708342122188157, -8.991547236680613508 ) ) ;
#13719 = CARTESIAN_POINT ( 'NONE',  ( -11.49634864345504148, 10.00000000000000711, -4.013552247486381397 ) ) ;
#13720 = CARTESIAN_POINT ( 'NONE',  ( -9.552639591052204498E-13, -45.78749999999988773, 11.37500000000000000 ) ) ;
#13721 = AXIS2_PLACEMENT_3D ( 'NONE', #606, #10085, #15435 ) ;
#13722 = CARTESIAN_POINT ( 'NONE',  ( -8.343458848123578520, 51.47999999999998977, -11.48378591275254124 ) ) ;
#13723 = CARTESIAN_POINT ( 'NONE',  ( 13.50075696862491270, 33.43493226266512153, -0.1459511389326202946 ) ) ;
#13724 = CARTESIAN_POINT ( 'NONE',  ( 1.785599194582236620E-06, 38.68004968046676595, 13.49999999999976374 ) ) ;
#13725 = ORIENTED_EDGE ( 'NONE', *, *, #7415, .T. ) ;
#13726 = ORIENTED_EDGE ( 'NONE', *, *, #17449, .T. ) ;
#13727 = CARTESIAN_POINT ( 'NONE',  ( -5.547022999642051033, 62.47876125775495382, 12.30782497079059112 ) ) ;
#13728 = EDGE_LOOP ( 'NONE', ( #13641, #13111, #15522, #9243 ) ) ;
#13729 = CARTESIAN_POINT ( 'NONE',  ( 9.520470885617715595, -15.86999999999999567, 6.917026985038135400 ) ) ;
#13730 = CARTESIAN_POINT ( 'NONE',  ( 7.714727599197340524, -20.77812499999997087, 18.62500000000063949 ) ) ;
#13731 = CARTESIAN_POINT ( 'NONE',  ( -13.45405233132106559, 43.89143693887756115, -1.114340582890286147 ) ) ;
#13732 = CARTESIAN_POINT ( 'NONE',  ( -10.18076046065006146, 7.956441901775577641, 15.32106749056508299 ) ) ;
#13733 = EDGE_CURVE ( 'NONE', #17339, #10469, #143, .T. ) ;
#13734 = CARTESIAN_POINT ( 'NONE',  ( 8.343458848123583849, 36.88000000000000256, -11.48378591275253768 ) ) ;
#13735 = CARTESIAN_POINT ( 'NONE',  ( 7.714727599197340524, -56.22812499999984936, 18.62500000000063949 ) ) ;
#13736 = CARTESIAN_POINT ( 'NONE',  ( -11.33016873246668332, 67.65477934096038837, -7.343225168427664151 ) ) ;
#13737 = CARTESIAN_POINT ( 'NONE',  ( 13.16986379959833897, -90.56874999999976694, 13.16986379960055409 ) ) ;
#13738 = CARTESIAN_POINT ( 'NONE',  ( 13.04221433085913162, 54.30570824892984660, 3.485897513213817245 ) ) ;
#13739 = CARTESIAN_POINT ( 'NONE',  ( -5.921537691333334408, 64.39584764108268189, -12.13204556011841717 ) ) ;
#13740 = ORIENTED_EDGE ( 'NONE', *, *, #13690, .T. ) ;
#13741 = CARTESIAN_POINT ( 'NONE',  ( -12.97726217643209523, 34.79696272453640660, -3.720529569677623716 ) ) ;
#13742 = ORIENTED_EDGE ( 'NONE', *, *, #1488, .T. ) ;
#13743 = CARTESIAN_POINT ( 'NONE',  ( 12.93099675800281290, 78.29102732052795943, 3.879033096742795728 ) ) ;
#13744 = CARTESIAN_POINT ( 'NONE',  ( -10.35198169125275847, 7.925746654722171769, -15.34401010674823240 ) ) ;
#13745 = CARTESIAN_POINT ( 'NONE',  ( 7.500000000000000888, -27.00941661075428613, -5.548846425319421627 ) ) ;
#13746 = CARTESIAN_POINT ( 'NONE',  ( 7.461391812952430591, 72.90074887590216690, -11.25360145054118099 ) ) ;
#13747 = CARTESIAN_POINT ( 'NONE',  ( 1.323381335176092133, 79.13244564980092832, -13.43676060346282419 ) ) ;
#13748 = ADVANCED_FACE ( 'NONE', ( #11370 ), #16742, .T. ) ;
#13749 = CARTESIAN_POINT ( 'NONE',  ( 6.750017152462248760, -20.07073847365936814, 11.69133304809444773 ) ) ;
#13750 = CARTESIAN_POINT ( 'NONE',  ( -4.171729424061787483, 61.32999999999999829, -12.83926296998457417 ) ) ;
#13751 = CARTESIAN_POINT ( 'NONE',  ( -12.75901118186940586, 52.77091922838527438, -4.411226007631005253 ) ) ;
#13752 = CARTESIAN_POINT ( 'NONE',  ( -11.76794919243112325, 42.08000000000000540, 3.823638476888994386 ) ) ;
#13753 = CARTESIAN_POINT ( 'NONE',  ( -4.171729424061787483, 60.32999999999999829, -12.83926296998457417 ) ) ;
#13754 = CARTESIAN_POINT ( 'NONE',  ( -15.34492079894883965, 7.924935932049796072, -10.35602470258078789 ) ) ;
#13755 = CARTESIAN_POINT ( 'NONE',  ( 10.00829467491076485, 69.07965399636564996, 9.060027076871868701 ) ) ;
#13756 = CARTESIAN_POINT ( 'NONE',  ( 7.416407864998753041, 2.113974596215577595, 10.20780970022449985 ) ) ;
#13757 = CARTESIAN_POINT ( 'NONE',  ( 0.8900087425982343703, 35.71200196797583715, 13.47797884115083100 ) ) ;
#13758 = CARTESIAN_POINT ( 'NONE',  ( -18.62499999999935341, -64.48437499999987210, -7.714727599200458030 ) ) ;
#13759 = CARTESIAN_POINT ( 'NONE',  ( -13.00827088827464451, 74.05892661947035549, 3.610402901760149330 ) ) ;
#13760 = CARTESIAN_POINT ( 'NONE',  ( -7.025205504711061977, 76.44071120418792020, -11.52839822497519151 ) ) ;
#13761 = CARTESIAN_POINT ( 'NONE',  ( 17.32050807568873552, 7.773118517290098062, 8.000000000000083489 ) ) ;
#13762 = CARTESIAN_POINT ( 'NONE',  ( 7.347880794884122694E-16, 0.000000000000000000, -20.00000000000000000 ) ) ;
#13763 = CARTESIAN_POINT ( 'NONE',  ( -6.155833696462079452, 80.93000000000004945, 11.06015457064189533 ) ) ;
#13764 = CARTESIAN_POINT ( 'NONE',  ( -7.272992578804307939, -8.520000000000001350, -10.01041549318726886 ) ) ;
#13765 = CARTESIAN_POINT ( 'NONE',  ( 7.272992578804308828, 36.97999999999998977, 10.01041549318726886 ) ) ;
#13766 = CARTESIAN_POINT ( 'NONE',  ( 7.499999999999998224, 88.93000000000000682, -9.367496997597600128 ) ) ;
#13767 = CARTESIAN_POINT ( 'NONE',  ( -7.404169159380166398, 32.40321505951770575, 11.28896134248388172 ) ) ;
#13768 = CARTESIAN_POINT ( 'NONE',  ( 12.25829416376886449, 75.22281960573182857, 5.655528820242253119 ) ) ;
#13769 = ADVANCED_FACE ( 'NONE', ( #14175 ), #10224, .T. ) ;
#13770 = CARTESIAN_POINT ( 'NONE',  ( 3.371388833146295116, 7.495012466571698890E-16, -13.77928291208580980 ) ) ;
#13771 = CIRCLE ( 'NONE', #4762, 26.00000000000000355 ) ;
#13772 =( LENGTH_UNIT ( ) NAMED_UNIT ( * ) SI_UNIT ( .MILLI., .METRE. ) );
#13773 = CARTESIAN_POINT ( 'NONE',  ( 10.92172942406178926, 83.13000000000000966, 7.935100905948387684 ) ) ;
#13774 = CARTESIAN_POINT ( 'NONE',  ( 1.604790158072814110, 52.12231609098622442, -13.40787048747939814 ) ) ;
#13775 = CARTESIAN_POINT ( 'NONE',  ( -1.526447249548634533, 38.62512138167515729, 13.41343178257564439 ) ) ;
#13776 = CARTESIAN_POINT ( 'NONE',  ( 0.03713345166139490200, 37.17866481807171652, -13.49999999999999822 ) ) ;
#13777 = CARTESIAN_POINT ( 'NONE',  ( -12.00000000000002842, 1.213974596215577906, 3.899036354794884307 ) ) ;
#13778 = CARTESIAN_POINT ( 'NONE',  ( -8.891200544363830713E-16, 79.67999999999999261, 13.50000000000000000 ) ) ;
#13779 = CARTESIAN_POINT ( 'NONE',  ( 9.988255280523857138, 63.07858826136173036, 9.082801773783613086 ) ) ;
#13780 = CARTESIAN_POINT ( 'NONE',  ( 13.29809445833323345, 42.34812329220370941, 2.328726732125117937 ) ) ;
#13781 = CARTESIAN_POINT ( 'NONE',  ( 5.939848974692042205, 48.96343318860201776, -12.12304415933005508 ) ) ;
#13782 = AXIS2_PLACEMENT_3D ( 'NONE', #5706, #13716, #9686 ) ;
#13783 = CARTESIAN_POINT ( 'NONE',  ( 2.279995255611139653E-15, 21.17999999999998906, -12.37355403259654985 ) ) ;
#13784 = ORIENTED_EDGE ( 'NONE', *, *, #17109, .T. ) ;
#13785 = CARTESIAN_POINT ( 'NONE',  ( -3.636496289402153081, 80.32999999999999829, -11.19198476289190936 ) ) ;
#13786 = CARTESIAN_POINT ( 'NONE',  ( -2.557941946237081154, 70.27197374004576602, -13.25546265980607430 ) ) ;
#13787 = CARTESIAN_POINT ( 'NONE',  ( -11.37499999999960387, -73.88437499999982094, -4.711679271994911211 ) ) ;
#13788 = CARTESIAN_POINT ( 'NONE',  ( 4.171729424061789260, 5.830000000000001847, 12.83926296998457239 ) ) ;
#13789 = ORIENTED_EDGE ( 'NONE', *, *, #14312, .T. ) ;
#13790 = CARTESIAN_POINT ( 'NONE',  ( -10.73012146010035650, 43.61871145852727949, -8.197739046590561074 ) ) ;
#13791 = CARTESIAN_POINT ( 'NONE',  ( -7.499999999999998224, 108.3768542179258247, 4.091673783487171256 ) ) ;
#13792 = CARTESIAN_POINT ( 'NONE',  ( 13.48476133616894579, 60.45297963137706176, -0.6663839570962580838 ) ) ;
#13793 = CARTESIAN_POINT ( 'NONE',  ( 2.621994543952811015E-15, 5.180000000000002380, -14.19474002721660355 ) ) ;
#13794 = EDGE_CURVE ( 'NONE', #2328, #3933, #1459, .T. ) ;
#13795 = DIRECTION ( 'NONE',  ( 0.000000000000000000, 0.000000000000000000, -1.000000000000000000 ) ) ;
#13796 = CARTESIAN_POINT ( 'NONE',  ( 11.80065256636056148, 66.18689098013105365, 6.557030243741954756 ) ) ;
#13797 = CARTESIAN_POINT ( 'NONE',  ( 3.282856408315379504, 56.79801877443869529, 13.09476614375152259 ) ) ;
#13798 = CARTESIAN_POINT ( 'NONE',  ( -11.76794919243112325, 60.07999999999999119, 3.823638476888994386 ) ) ;
#13799 = CARTESIAN_POINT ( 'NONE',  ( -9.520470885617715595, 62.63000000000000256, -6.917026985038136289 ) ) ;
#13800 = CARTESIAN_POINT ( 'NONE',  ( -13.50037362800620322, 46.92666714195863875, -0.09336111851946382600 ) ) ;
#13801 = AXIS2_PLACEMENT_3D ( 'NONE', #10550, #6828, #13610 ) ;
#13802 = CARTESIAN_POINT ( 'NONE',  ( 11.80278193115546159, 45.67295468282410553, -6.553216385568251923 ) ) ;
#13803 = DIRECTION ( 'NONE',  ( -0.000000000000000000, -1.000000000000000000, -0.000000000000000000 ) ) ;
#13804 = FILL_AREA_STYLE ('',( #3019 ) ) ;
#13805 = CARTESIAN_POINT ( 'NONE',  ( 0.9194697767184354387, 31.14698203856080383, -13.46990214303131239 ) ) ;
#13806 = CARTESIAN_POINT ( 'NONE',  ( -3.615283074269553865, 56.54999604154088644, 13.00706333399712378 ) ) ;
#13807 = CARTESIAN_POINT ( 'NONE',  ( -11.37500000000000000, -74.92499999999982663, -9.545674412382054647E-13 ) ) ;
#13808 = CARTESIAN_POINT ( 'NONE',  ( -8.343458848123582072, 52.37999999999999545, 11.48378591275253768 ) ) ;
#13809 = CARTESIAN_POINT ( 'NONE',  ( 6.559526086243817389, 32.92132783700705545, 11.80121481743272582 ) ) ;
#13810 = CARTESIAN_POINT ( 'NONE',  ( -15.58845726811976817, 0.000000000000000000, -11.00000000000018296 ) ) ;
#13811 = SURFACE_STYLE_FILL_AREA ( #3589 ) ;
#13812 = ORIENTED_EDGE ( 'NONE', *, *, #11260, .F. ) ;
#13813 = CARTESIAN_POINT ( 'NONE',  ( -13.46388178117166667, 61.96414966410978309, 0.9868924404964516395 ) ) ;
#13814 = VERTEX_POINT ( 'NONE', #1973 ) ;
#13815 = CARTESIAN_POINT ( 'NONE',  ( 18.62500000000064659, -74.89062499999985789, -7.714727599197336083 ) ) ;
#13816 = CARTESIAN_POINT ( 'NONE',  ( -13.15137912863705694, 43.81956125819836245, -3.114482827138729260 ) ) ;
#13817 = CARTESIAN_POINT ( 'NONE',  ( 2.445080149700053643E-15, 4.180000000000004157, -13.50000000000000000 ) ) ;
#13818 = CARTESIAN_POINT ( 'NONE',  ( -11.76794919243112325, 83.93000000000000682, -2.882316262207890869E-15 ) ) ;
#13819 = CARTESIAN_POINT ( 'NONE',  ( -4.433696007799730054, 46.33947026150794812, -12.75186962703676308 ) ) ;
#13820 = CARTESIAN_POINT ( 'NONE',  ( -2.946493560005031487, 67.28594004907910175, -13.17452797624288507 ) ) ;
#13821 = CARTESIAN_POINT ( 'NONE',  ( 13.16986379960055409, -78.08124999999978400, -13.16986379959834430 ) ) ;
#13822 = CARTESIAN_POINT ( 'NONE',  ( 9.472162392857283564, 54.05224036424414891, 9.619202640402704674 ) ) ;
#13823 = EDGE_CURVE ( 'NONE', #2328, #7389, #6328, .T. ) ;
#13824 = CARTESIAN_POINT ( 'NONE',  ( -6.457592974018579568, 64.41724210666654926, -11.85949774483797015 ) ) ;
#13825 = ORIENTED_EDGE ( 'NONE', *, *, #5848, .F. ) ;
#13826 = CARTESIAN_POINT ( 'NONE',  ( 16.17460542229563814, 8.007813505529846054, -8.351563113033689589 ) ) ;
#13827 = CARTESIAN_POINT ( 'NONE',  ( -10.19687314292181490, 34.58963878807200132, -8.847247010019716029 ) ) ;
#13828 = CARTESIAN_POINT ( 'NONE',  ( -11.37500000000039613, -59.31562499999985505, 4.711679271993002516 ) ) ;
#13829 = ORIENTED_EDGE ( 'NONE', *, *, #3626, .F. ) ;
#13830 = CARTESIAN_POINT ( 'NONE',  ( 11.22821437167453951, 78.14808671973084131, 7.504731954664256577 ) ) ;
#13831 = FACE_OUTER_BOUND ( 'NONE', #10316, .T. ) ;
#13832 = AXIS2_PLACEMENT_3D ( 'NONE', #3126, #15137, #3034 ) ;
#13833 = CARTESIAN_POINT ( 'NONE',  ( 12.72858050653801243, 72.26759830117254069, 4.498419153570456963 ) ) ;
#13834 = CARTESIAN_POINT ( 'NONE',  ( 7.157097987683219920, 78.91372639992512461, -11.44668968571802914 ) ) ;
#13835 = CARTESIAN_POINT ( 'NONE',  ( 10.92172942406179104, -19.27000000000000313, -7.935100905948385908 ) ) ;
#13836 = CARTESIAN_POINT ( 'NONE',  ( 4.171729424061791924, 61.03000000000000114, -12.83926296998457239 ) ) ;
#13837 = CARTESIAN_POINT ( 'NONE',  ( -12.72397836871632570, 52.76708174372507898, -4.512114305315815699 ) ) ;
#13838 = CARTESIAN_POINT ( 'NONE',  ( 3.636496289402157078, 38.03000000000000114, -11.19198476289190936 ) ) ;
#13839 = CARTESIAN_POINT ( 'NONE',  ( 4.171729424061789260, 61.82999999999999829, 12.83926296998457417 ) ) ;
#13840 = CARTESIAN_POINT ( 'NONE',  ( -8.224360503536546367E-15, 78.17999999999999261, -13.50000000000000000 ) ) ;
#13841 = CARTESIAN_POINT ( 'NONE',  ( 3.636496289402157078, -5.969999999999996199, -11.19198476289190936 ) ) ;
#13842 = CARTESIAN_POINT ( 'NONE',  ( 6.937372977335349411, 68.93680969837741657, 11.59389707275178516 ) ) ;
#13843 = CARTESIAN_POINT ( 'NONE',  ( -2.773849517010688714, 37.27973736289535367, -13.21200723427060275 ) ) ;
#13844 = DIRECTION ( 'NONE',  ( 1.426480712616743416E-14, 0.000000000000000000, -1.000000000000000000 ) ) ;
#13845 = CARTESIAN_POINT ( 'NONE',  ( 18.62500000000000000, -90.49999999999980105, 1.560692158462880521E-12 ) ) ;
#13846 = CARTESIAN_POINT ( 'NONE',  ( -12.66327544140950323, 73.76069652301814017, -4.679031621454643464 ) ) ;
#13847 = CARTESIAN_POINT ( 'NONE',  ( -2.436128718453049125, 76.26759188019981650, -13.27840869175127558 ) ) ;
#13848 = CARTESIAN_POINT ( 'NONE',  ( 6.123233995736766282E-16, 73.00000000000001421, 5.000000000000000000 ) ) ;
#13849 = DIRECTION ( 'NONE',  ( -0.000000000000000000, 1.000000000000000000, -0.000000000000000000 ) ) ;
#13850 = CARTESIAN_POINT ( 'NONE',  ( -13.49999999999999822, 30.07999999999999829, 4.386415899144235908 ) ) ;
#13851 = CARTESIAN_POINT ( 'NONE',  ( -9.520470885617717371, -7.769999999999999574, 6.917026985038133624 ) ) ;
#13852 = CARTESIAN_POINT ( 'NONE',  ( 7.272992578804308828, 39.97999999999999687, 10.01041549318726886 ) ) ;
#13853 = CARTESIAN_POINT ( 'NONE',  ( 9.708203932499371192, 5.863974596215575374, -7.053423027509676757 ) ) ;
#13854 = CARTESIAN_POINT ( 'NONE',  ( -7.866632585845692915, 32.38327360912128938, 10.98016383686059072 ) ) ;
#13855 = CARTESIAN_POINT ( 'NONE',  ( 13.23619622236415694, 75.33619659209034580, 2.658123818869813970 ) ) ;
#13856 = CARTESIAN_POINT ( 'NONE',  ( 14.83981042559783425, 2.881527793022525794E-15, -10.59219708354840250 ) ) ;
#13857 = CARTESIAN_POINT ( 'NONE',  ( 12.00000000000000533, 94.93000000000002103, 1.224646799147353059E-15 ) ) ;
#13858 = CARTESIAN_POINT ( 'NONE',  ( 3.636496289402157078, 32.02999999999999403, -11.19198476289190936 ) ) ;
#13859 = CARTESIAN_POINT ( 'NONE',  ( -2.360907066372419649, 58.26488951066585287, -13.29195769039779762 ) ) ;
#13860 = CYLINDRICAL_SURFACE ( 'NONE', #1094, 1.999999999999998224 ) ;
#13861 = CARTESIAN_POINT ( 'NONE',  ( 0.1099142029571859580, 37.17604789069145710, -13.49955337541945610 ) ) ;
#13862 = EDGE_CURVE ( 'NONE', #6926, #3781, #6706, .T. ) ;
#13863 = DIRECTION ( 'NONE',  ( 0.000000000000000000, -1.000000000000000000, 0.000000000000000000 ) ) ;
#13864 = EDGE_CURVE ( 'NONE', #5695, #14678, #8529, .T. ) ;
#13865 = CARTESIAN_POINT ( 'NONE',  ( -0.01835916714045033107, 49.18066010337725658, -13.49998829627290675 ) ) ;
#13866 = CARTESIAN_POINT ( 'NONE',  ( 9.659554295284692671, 63.06166812284966028, 9.431042181653399581 ) ) ;
#13867 = CARTESIAN_POINT ( 'NONE',  ( 13.48976328056408747, 42.44825124965819185, -0.5305257734362035515 ) ) ;
#13868 = CARTESIAN_POINT ( 'NONE',  ( 13.40726971276752799, 48.37312214362100349, 1.632088562652946662 ) ) ;
#13869 = CARTESIAN_POINT ( 'NONE',  ( 11.76794919243112325, 20.43000000000000327, 1.734723475976807094E-15 ) ) ;
#13870 = EDGE_LOOP ( 'NONE', ( #5007, #6409 ) ) ;
#13871 = CARTESIAN_POINT ( 'NONE',  ( -9.520470885617715595, 65.62999999999999545, -6.917026985038136289 ) ) ;
#13872 = DIRECTION ( 'NONE',  ( 0.5000000000000007772, 0.000000000000000000, 0.8660254037844381525 ) ) ;
#13873 = CARTESIAN_POINT ( 'NONE',  ( 11.37500000000000000, -66.59999999999983800, 9.531744055041752924E-13 ) ) ;
#13874 = CARTESIAN_POINT ( 'NONE',  ( 13.50000000000000355, 6.580000000000001847, -4.386415899144233244 ) ) ;
#13875 = ORIENTED_EDGE ( 'NONE', *, *, #3600, .T. ) ;
#13876 = CARTESIAN_POINT ( 'NONE',  ( -12.58667385456655552, 43.75263158861623225, -4.890129452139457378 ) ) ;
#13877 = DIRECTION ( 'NONE',  ( -0.000000000000000000, 1.000000000000000000, -0.000000000000000000 ) ) ;
#13878 = CARTESIAN_POINT ( 'NONE',  ( -10.92172942406178926, 5.629999999999996341, -7.935100905948389460 ) ) ;
#13879 = DIRECTION ( 'NONE',  ( 0.000000000000000000, -1.000000000000000000, 0.000000000000000000 ) ) ;
#13880 = CARTESIAN_POINT ( 'NONE',  ( 10.75445589294585425, 66.11967042978940867, 8.172061559770561701 ) ) ;
#13881 = CARTESIAN_POINT ( 'NONE',  ( 9.434980010212051127, 57.05010519921826528, 9.665379090820270136 ) ) ;
#13882 = CARTESIAN_POINT ( 'NONE',  ( 7.272992578804308828, 63.97999999999998977, 10.01041549318726709 ) ) ;
#13883 = CARTESIAN_POINT ( 'NONE',  ( -13.49999999999999822, 33.77999999999998693, -4.386415899144240349 ) ) ;
#13884 = CARTESIAN_POINT ( 'NONE',  ( -9.520470885617715595, 65.62999999999999545, -6.917026985038136289 ) ) ;
#13885 = VECTOR ( 'NONE', #3573, 1000.000000000000000 ) ;
#13886 = CARTESIAN_POINT ( 'NONE',  ( -11.35984435782789248, 46.65678690620720204, -7.294136646755872810 ) ) ;
#13887 = CARTESIAN_POINT ( 'NONE',  ( 8.617250736976671988, 45.84912361920483193, -10.39756555118851722 ) ) ;
#13888 = CARTESIAN_POINT ( 'NONE',  ( 0.2178731047108220797, 70.17216608048821058, -13.49830902344535488 ) ) ;
#13889 =( NAMED_UNIT ( * ) PLANE_ANGLE_UNIT ( ) SI_UNIT ( $, .RADIAN. ) );
#13890 = CARTESIAN_POINT ( 'NONE',  ( 10.44099705197275973, 30.75714436294632748, -8.557786488581344386 ) ) ;
#13891 = CARTESIAN_POINT ( 'NONE',  ( -2.103740194764985638, 56.60437523833922313, 13.33510591258322009 ) ) ;
#13892 = CARTESIAN_POINT ( 'NONE',  ( 13.49999999999999822, 53.27999999999999403, 4.386415899144236796 ) ) ;
#13893 = CARTESIAN_POINT ( 'NONE',  ( 5.991907069272227382, 32.89832976177464019, 12.10500988212866780 ) ) ;
#13894 = DIRECTION ( 'NONE',  ( -0.4999999999999882316, 0.000000000000000000, -0.8660254037844454800 ) ) ;
#13895 = CARTESIAN_POINT ( 'NONE',  ( 2.448403087673295619, 40.09219290737040353, -13.28282402178302135 ) ) ;
#13896 = CARTESIAN_POINT ( 'NONE',  ( 2.279995255611139653E-15, 24.17999999999999261, -12.37355403259654985 ) ) ;
#13897 = VERTEX_POINT ( 'NONE', #5352 ) ;
#13898 = CARTESIAN_POINT ( 'NONE',  ( -13.47307933246733214, 61.90057393254070206, -0.8523656554613193714 ) ) ;
#13899 = EDGE_LOOP ( 'NONE', ( #8631, #6337, #5207, #9784 ) ) ;
#13900 = AXIS2_PLACEMENT_3D ( 'NONE', #12734, #10268, #621 ) ;
#13901 = CARTESIAN_POINT ( 'NONE',  ( 7.272992578804308828, -16.02000000000000313, 10.01041549318726709 ) ) ;
#13902 = CARTESIAN_POINT ( 'NONE',  ( 7.714727599197340524, -54.07812499999989342, 18.62500000000063949 ) ) ;
#13903 = CARTESIAN_POINT ( 'NONE',  ( -11.06759828328972262, 44.22140378436495922, 7.730498622152057742 ) ) ;
#13904 = CARTESIAN_POINT ( 'NONE',  ( 4.171729424061789260, 64.82999999999999829, 12.83926296998457417 ) ) ;
#13905 = CARTESIAN_POINT ( 'NONE',  ( 4.171729424061791924, 37.03000000000000114, -12.83926296998457239 ) ) ;
#13906 =( BOUNDED_CURVE ( )  B_SPLINE_CURVE ( 2, ( #13175, #6560, #17321, #1232, #16244 ),
 .UNSPECIFIED., .F., .F. ) 
 B_SPLINE_CURVE_WITH_KNOTS ( ( 3, 2, 3 ),
 ( 0.4326563348871274028, 0.4358520785730354841, 0.4386822870511441486 ),
 .UNSPECIFIED. ) 
 CURVE ( )  GEOMETRIC_REPRESENTATION_ITEM ( )  RATIONAL_B_SPLINE_CURVE ( ( 0.9759364712373530537, 0.9723676117969409782, 1.000000000000000000, 0.9755282566284837475, 0.9755282581475768211 ) ) 
 REPRESENTATION_ITEM ( '' )  );
#13907 = CARTESIAN_POINT ( 'NONE',  ( -9.622267015188688433, 46.55978118158259349, -9.469001082431288907 ) ) ;
#13908 = CARTESIAN_POINT ( 'NONE',  ( -1.537544760673846822, 67.23529664120425764, -13.41438453500880890 ) ) ;
#13909 = CARTESIAN_POINT ( 'NONE',  ( 11.37500000000039613, 6.209375000000004974, -4.711679271993004292 ) ) ;
#13910 = EDGE_CURVE ( 'NONE', #5991, #11898, #9342, .T. ) ;
#13911 = CARTESIAN_POINT ( 'NONE',  ( 7.231211556383717820, 53.94958124039511915, 11.40216215182779180 ) ) ;
#13912 = ORIENTED_EDGE ( 'NONE', *, *, #16694, .T. ) ;
#13913 = CARTESIAN_POINT ( 'NONE',  ( -9.971648473084066211, 64.57780736460058790, -9.102418965360820735 ) ) ;
#13914 = ORIENTED_EDGE ( 'NONE', *, *, #4815, .T. ) ;
#13915 = CARTESIAN_POINT ( 'NONE',  ( 13.50000000000000355, 9.580000000000008953, -4.386415899144233244 ) ) ;
#13916 = CARTESIAN_POINT ( 'NONE',  ( -10.18520613440925082, 34.58903015065802578, -8.860683611510044244 ) ) ;
#13917 = CARTESIAN_POINT ( 'NONE',  ( 8.043339635997654113, -35.38124999999991616, -8.043339635996304082 ) ) ;
#13918 = CARTESIAN_POINT ( 'NONE',  ( 13.21851051443945479, 78.52727199688872872, -2.752770575687411014 ) ) ;
#13919 = DIRECTION ( 'NONE',  ( -1.927470528863120035E-16, 1.000000000000000000, 0.000000000000000000 ) ) ;
#13920 = CARTESIAN_POINT ( 'NONE',  ( 7.500000000000001776, -23.75733333946869408, 9.035253535952435300 ) ) ;
#13921 = CARTESIAN_POINT ( 'NONE',  ( 11.49807445461734012, 72.16584275115400260, 7.074230165436003581 ) ) ;
#13922 = CARTESIAN_POINT ( 'NONE',  ( -11.76794919243112325, 27.93000000000001037, -2.602085213965210642E-15 ) ) ;
#13923 = CARTESIAN_POINT ( 'NONE',  ( -10.92172942406178926, 61.63000000000000256, -7.935100905948389460 ) ) ;
#13924 = CARTESIAN_POINT ( 'NONE',  ( -1.421510037799555759, 71.62891323700581836, 13.42697251540404757 ) ) ;
#13925 = CARTESIAN_POINT ( 'NONE',  ( -11.76794919243112325, 41.92999999999999261, -2.882316262207890869E-15 ) ) ;
#13926 = CARTESIAN_POINT ( 'NONE',  ( 4.171729424061789260, 55.83000000000000540, 12.83926296998457417 ) ) ;
#13927 = CARTESIAN_POINT ( 'NONE',  ( -16.97734196418681307, 7.854010772509913529, -8.022095340454654888 ) ) ;
#13928 = CARTESIAN_POINT ( 'NONE',  ( 2.279995255611139653E-15, 0.1800000000000001044, -12.37355403259654985 ) ) ;
#13929 = CARTESIAN_POINT ( 'NONE',  ( 8.535454704214165744, 69.00715068001011332, 10.46229327927559183 ) ) ;
#13930 = CARTESIAN_POINT ( 'NONE',  ( 1.900613283894512451, 1.890856018535849392, 12.00000000000000000 ) ) ;
#13931 = CARTESIAN_POINT ( 'NONE',  ( 1.363617428356367123, 35.72903063807564195, 13.43096419532364294 ) ) ;
#13932 = CARTESIAN_POINT ( 'NONE',  ( -18.62500000000000000, -48.87499999999990052, -1.562973063126292757E-12 ) ) ;
#13933 = CARTESIAN_POINT ( 'NONE',  ( -13.48837046896241354, 73.91067174755934843, -0.5608890242489086297 ) ) ;
#13934 = CARTESIAN_POINT ( 'NONE',  ( -1.732050807569007977, 0.000000000000000000, 18.99999999999998224 ) ) ;
#13935 = DIRECTION ( 'NONE',  ( 4.676985943005715098E-16, -0.000000000000000000, 1.000000000000000000 ) ) ;
#13936 = DIRECTION ( 'NONE',  ( -1.000000000000000000, -0.000000000000000000, -0.000000000000000000 ) ) ;
#13937 = DIRECTION ( 'NONE',  ( 0.000000000000000000, 0.000000000000000000, 1.000000000000000000 ) ) ;
#13938 = SURFACE_STYLE_FILL_AREA ( #4240 ) ;
#13939 = CARTESIAN_POINT ( 'NONE',  ( -11.76794919243112325, -8.220000000000004192, -3.823638476888998827 ) ) ;
#13940 = CARTESIAN_POINT ( 'NONE',  ( 11.76794919243112680, 34.57999999999999829, -3.823638476888993942 ) ) ;
#13941 = CARTESIAN_POINT ( 'NONE',  ( -13.49999999999999822, 1.780000000000000471, -4.386415899144240349 ) ) ;
#13942 = CARTESIAN_POINT ( 'NONE',  ( -6.679390041561677371, 32.43370277562137005, 11.73465909257911832 ) ) ;
#13943 = CARTESIAN_POINT ( 'NONE',  ( 1.329527900993174860, 74.72780491797803393, 13.43437217338847844 ) ) ;
#13944 = CARTESIAN_POINT ( 'NONE',  ( -0.08605353725393936892, 53.67690303198914847, 13.49999999999942091 ) ) ;
#13945 = DIRECTION ( 'NONE',  ( 1.000000000000000000, 0.000000000000000000, 0.000000000000000000 ) ) ;
#13946 = CARTESIAN_POINT ( 'NONE',  ( -8.343458848123576743, 81.48000000000000398, -11.48378591275254301 ) ) ;
#13947 = VECTOR ( 'NONE', #6433, 1000.000000000000000 ) ;
#13948 = CARTESIAN_POINT ( 'NONE',  ( 4.710692427101017543, 52.01035291496985025, -12.65147037080429726 ) ) ;
#13949 = CARTESIAN_POINT ( 'NONE',  ( -2.093142125047454449, 38.60467073819259554, 13.33804731820490552 ) ) ;
#13950 = DIRECTION ( 'NONE',  ( -0.000000000000000000, 1.000000000000000000, -0.000000000000000000 ) ) ;
#13951 = CARTESIAN_POINT ( 'NONE',  ( -8.891200544363830713E-16, 70.68000000000000682, 13.50000000000000000 ) ) ;
#13952 = CARTESIAN_POINT ( 'NONE',  ( -0.06416183230854911879, 49.18230675135094287, -13.49986922154364777 ) ) ;
#13953 = CARTESIAN_POINT ( 'NONE',  ( 10.66583021020285393, 63.11535396121603725, 8.275874897226483284 ) ) ;
#13954 = CARTESIAN_POINT ( 'NONE',  ( 7.562216151199702807, 41.96360496807130858, 11.18639152389247471 ) ) ;
#13955 = CARTESIAN_POINT ( 'NONE',  ( 12.27263252356545209, 48.63596850838850116, -5.624294195753364534 ) ) ;
#13956 = CARTESIAN_POINT ( 'NONE',  ( 3.636496289402154414, 22.83000000000001606, 11.19198476289190758 ) ) ;
#13957 = ORIENTED_EDGE ( 'NONE', *, *, #12169, .F. ) ;
#13958 = CARTESIAN_POINT ( 'NONE',  ( -9.520470885617715595, 68.62999999999999545, -6.917026985038136289 ) ) ;
#13959 = CARTESIAN_POINT ( 'NONE',  ( -11.37500000000000178, -17.72499999999994102, -9.545674412382054647E-13 ) ) ;
#13960 = CARTESIAN_POINT ( 'NONE',  ( 4.711679271993006068, -63.47812499999984226, 11.37500000000039257 ) ) ;
#13961 = CARTESIAN_POINT ( 'NONE',  ( -10.92172942406179104, 8.230000000000014637, 7.935100905948385908 ) ) ;
#13962 = ORIENTED_EDGE ( 'NONE', *, *, #17013, .T. ) ;
#13963 = CARTESIAN_POINT ( 'NONE',  ( -0.3404806211656328241, 43.19224228718480418, -13.49585535663135794 ) ) ;
#13964 = CARTESIAN_POINT ( 'NONE',  ( -2.522983078673279752E-14, 34.17999999999999972, -13.50000000000000000 ) ) ;
#13965 = CARTESIAN_POINT ( 'NONE',  ( 4.171729424061789260, 0.8299999999999974065, 12.83926296998457239 ) ) ;
#13966 = CARTESIAN_POINT ( 'NONE',  ( -18.62499999999935341, -7.284374999999982947, -7.714727599200458918 ) ) ;
#13967 = CARTESIAN_POINT ( 'NONE',  ( 10.23380095822083291, 66.09158251474292456, 8.804547898461850153 ) ) ;
#13968 = CARTESIAN_POINT ( 'NONE',  ( -4.171729424061787483, 79.32999999999999829, -12.83926296998457417 ) ) ;
#13969 = ADVANCED_FACE ( 'NONE', ( #2666 ), #13121, .F. ) ;
#13970 = AXIS2_PLACEMENT_3D ( 'NONE', #1125, #7948, #6622 ) ;
#13971 = CARTESIAN_POINT ( 'NONE',  ( -7.272992578804310604, 57.37999999999998835, 10.01041549318726709 ) ) ;
#13972 = CARTESIAN_POINT ( 'NONE',  ( 2.272985001014427788E-15, 62.17999999999999972, -12.37355403259654985 ) ) ;
#13973 = CARTESIAN_POINT ( 'NONE',  ( -11.41968976572175976, 46.66065175804080667, -7.200595652070090225 ) ) ;
#13974 = CARTESIAN_POINT ( 'NONE',  ( 10.84045915709670993, 45.73470465951034214, -8.047803413914586201 ) ) ;
#13975 = CARTESIAN_POINT ( 'NONE',  ( 8.035699651468419802, 69.87551396580593632, -10.84793394748052364 ) ) ;
#13976 = CARTESIAN_POINT ( 'NONE',  ( 8.184208372444009782, 30.86883944040518557, -10.73662710873863979 ) ) ;
#13977 = CARTESIAN_POINT ( 'NONE',  ( -13.46101982974745859, 55.96549097240059467, 1.025187530456345586 ) ) ;
#13978 = CARTESIAN_POINT ( 'NONE',  ( 0.000000000000000000, -22.00000000000000000, -6.000000000000001776 ) ) ;
#13979 = CARTESIAN_POINT ( 'NONE',  ( 1.852680671424132619, 32.74661364833260535, 13.38217953742864985 ) ) ;
#13980 = CARTESIAN_POINT ( 'NONE',  ( -7.499999999999998224, -8.000000000000000000, -9.367496997597607233 ) ) ;
#13981 = CARTESIAN_POINT ( 'NONE',  ( 11.36437994058350220, 39.70321145296029641, -7.292015817707691916 ) ) ;
#13982 = VERTEX_POINT ( 'NONE', #11804 ) ;
#13983 = CARTESIAN_POINT ( 'NONE',  ( -13.37679940684410163, 61.99543014590985734, 1.870821765799961733 ) ) ;
#13984 = VECTOR ( 'NONE', #11866, 1000.000000000000000 ) ;
#13985 = ORIENTED_EDGE ( 'NONE', *, *, #6292, .F. ) ;
#13986 = CARTESIAN_POINT ( 'NONE',  ( 7.272992578804311492, -18.12000000000000455, -10.01041549318726709 ) ) ;
#13987 = CARTESIAN_POINT ( 'NONE',  ( -7.714727599200466912, -51.99687499999990337, 18.62499999999935341 ) ) ;
#13988 = CARTESIAN_POINT ( 'NONE',  ( 11.03739991603106319, 48.13673635289907082, 7.779773485289230628 ) ) ;
#13989 = LINE ( 'NONE', #9965, #12146 ) ;
#13990 = CARTESIAN_POINT ( 'NONE',  ( -4.171729424061787483, 31.32999999999999829, -12.83926296998457417 ) ) ;
#13991 = CARTESIAN_POINT ( 'NONE',  ( 10.92172942406178926, 41.13000000000000256, 7.935100905948387684 ) ) ;
#13992 = EDGE_CURVE ( 'NONE', #7222, #11811, #12769, .T. ) ;
#13993 = VECTOR ( 'NONE', #3638, 999.9999999999998863 ) ;
#13994 = CARTESIAN_POINT ( 'NONE',  ( -3.342578662528335798, 46.30004703686991263, -13.08883371199211965 ) ) ;
#13995 = CARTESIAN_POINT ( 'NONE',  ( -0.03696684871921104842, 67.18132919150241378, -13.50000000000000000 ) ) ;
#13996 = CARTESIAN_POINT ( 'NONE',  ( -13.16986379960055409, -86.40624999999977263, 13.16986379959834252 ) ) ;
#13997 = CARTESIAN_POINT ( 'NONE',  ( 4.958073332672438660, 53.85884788343330598, 12.55661954819793635 ) ) ;
#13998 = CARTESIAN_POINT ( 'NONE',  ( 7.272992578804311492, 14.88000000000000078, -10.01041549318726709 ) ) ;
#13999 = EDGE_LOOP ( 'NONE', ( #14542, #9976, #1058, #17273 ) ) ;
#14000 = CARTESIAN_POINT ( 'NONE',  ( -10.99488771831293477, 64.63370636212923159, -7.845699068106005925 ) ) ;
#14001 = ORIENTED_EDGE ( 'NONE', *, *, #9656, .T. ) ;
#14002 = CARTESIAN_POINT ( 'NONE',  ( -2.734444271416374426E-11, 0.3139745962166686222, -12.00000000000000000 ) ) ;
#14003 = CARTESIAN_POINT ( 'NONE',  ( -8.055926233375233281, 34.48539140569977235, -10.83293180899966224 ) ) ;
#14004 = CARTESIAN_POINT ( 'NONE',  ( -8.043339635997654113, -27.05624999999993463, 8.043339635996302306 ) ) ;
#14005 = CARTESIAN_POINT ( 'NONE',  ( 10.45646361262144453, 78.10370444553853986, 8.538874148716518064 ) ) ;
#14006 = CARTESIAN_POINT ( 'NONE',  ( 8.343458848123583849, 47.87999999999999545, -11.48378591275253768 ) ) ;
#14007 = AXIS2_PLACEMENT_3D ( 'NONE', #17189, #14437, #13043 ) ;
#14008 = DIRECTION ( 'NONE',  ( -0.000000000000000000, -1.000000000000000000, -0.000000000000000000 ) ) ;
#14009 = CARTESIAN_POINT ( 'NONE',  ( 7.500000000000004441, -25.28385182205995818, -8.084116494856626645 ) ) ;
#14010 = CARTESIAN_POINT ( 'NONE',  ( 11.91517651397667699, 72.66463852654297284, -6.346540879243715239 ) ) ;
#14011 = CARTESIAN_POINT ( 'NONE',  ( 11.76794919243112325, 32.43000000000001393, 1.734723475976807094E-15 ) ) ;
#14012 =( BOUNDED_CURVE ( )  B_SPLINE_CURVE ( 2, ( #2427, #10510, #9697, #4198, #14540, #8283, #14867, #9522, #1356, #6863, #16471, #17208, #14961 ),
 .UNSPECIFIED., .F., .F. ) 
 B_SPLINE_CURVE_WITH_KNOTS ( ( 3, 2, 2, 2, 2, 2, 3 ),
 ( 0.7638888888888888395, 0.7666666666666667185, 0.7722222222222222543, 0.7777777777777777901, 0.7833333333333333259, 0.7888888888888888618, 0.7916666666666666297 ),
 .UNSPECIFIED. ) 
 CURVE ( )  GEOMETRIC_REPRESENTATION_ITEM ( )  RATIONAL_B_SPLINE_CURVE ( ( 0.9755282581475768211, 0.9755282581475762660, 1.000000000000000000, 0.9510565162951535312, 1.000000000000000000, 0.9510565162951535312, 1.000000000000000000, 0.9510565162951535312, 1.000000000000000000, 0.9510565162951535312, 1.000000000000000000, 0.9755282581475768211, 0.9755282581475768211 ) ) 
 REPRESENTATION_ITEM ( '' )  );
#14013 = CARTESIAN_POINT ( 'NONE',  ( -13.50000000000000000, 61.92999999999999972, -3.306546357697853733E-15 ) ) ;
#14014 = CARTESIAN_POINT ( 'NONE',  ( -8.629845922160509275, 52.51158210495129453, -10.38376407271738699 ) ) ;
#14015 = EDGE_CURVE ( 'NONE', #12574, #17443, #6571, .T. ) ;
#14016 = CARTESIAN_POINT ( 'NONE',  ( 3.636496289402154414, 36.82999999999999119, 11.19198476289190936 ) ) ;
#14017 = CARTESIAN_POINT ( 'NONE',  ( -3.636496289402152637, -14.66999999999999638, -11.19198476289190936 ) ) ;
#14018 = CARTESIAN_POINT ( 'NONE',  ( -4.171729424061791036, 55.52999999999999403, 12.83926296998457239 ) ) ;
#14019 = B_SPLINE_CURVE_WITH_KNOTS ( 'NONE', 3,
 ( #12238, #9694, #16289, #15042, #2938, #3118, #5890, #8367, #16469, #11097, #3026, #13895, #11184, #12418, #306, #5715, #7122, #4374, #1794, #16560, #9782, #4466, #15129, #8456, #7205, #16192, #3301, #3474, #13020, #14074, #16816, #8714, #12677, #16646, #11443, #2128, #9957, #7471, #3210, #8630, #7384, #1961, #740, #10125, #14159, #7292, #15305, #15478, #7643, #11356, #4552, #4724, #4808, #10210, #12762, #4637, #15393, #2047, #13981, #1877, #16990, #16730, #3389, #7554, #10044, #14327, #10295, #901, #567, #12851, #5974, #650, #6060, #12933, #8802, #6149, #11527, #16905, #15563, #8888, #14243, #817, #6228, #11614, #4894, #15647, #3557, #8971, #2216, #11269, #3993, #2647, #10720, #6660, #9237, #5249, #10635, #3733, #2300, #4979, #10555, #10382, #6403, #15736, #9323, #12041, #3645, #17075, #9059, #7904, #1248, #14412, #11786, #7728, #13104, #17250, #1167, #17420, #991, #3823, #17162, #15914, #5074, #1078, #10468, #15829, #9151, #14498, #2385, #7821, #5335, #8078, #13193, #6578, #11959, #16000, #16085, #2561, #6492, #11875, #5163, #14591, #17338, #9409, #2471, #13359, #14673, #13279, #3905, #7991, #14757, #13442, #6313, #11699, #4169, #6925, #16262, #2735, #6745, #1509, #9754, #105, #14932, #12125, #1597, #4079, #5690, #9581, #8341, #196, #4259, #14841, #5418, #5601, #15191, #1417, #14, #12302, #12390, #281, #2824 ),
 .UNSPECIFIED., .F., .F.,
 ( 4, 2, 1, 1, 1, 2, 2, 2, 2, 1, 2, 2, 1, 2, 2, 2, 2, 2, 2, 2, 1, 2, 2, 2, 2, 1, 1, 2, 2, 1, 1, 1, 1, 1, 2, 2, 2, 1, 2, 2, 1, 2, 2, 2, 2, 2, 2, 2, 1, 2, 2, 2, 1, 1, 1, 1, 2, 2, 2, 2, 2, 1, 2, 2, 1, 2, 2, 2, 2, 2, 1, 2, 2, 1, 1, 2, 2, 1, 1, 2, 2, 1, 2, 2, 2, 2, 2, 2, 1, 1, 2, 2, 2, 2, 2, 1, 1, 1, 2, 2, 2, 2, 2, 1, 1, 2, 2, 4 ),
 ( 0.7990296683925127708, 0.7990583905221522176, 0.7990871126517916645, 0.7991445569110705582, 0.7992594454296283457, 0.7994892224667439207, 0.7999487765409750706, 0.8008678846894373704, 0.8017869928378996702, 0.8020167698750152452, 0.8020742141342941389, 0.8021029362639335858, 0.8021316583935730327, 0.8022465469121308201, 0.8027061009863619701, 0.8036252091348243809, 0.8045443172832866807, 0.8050038713575178306, 0.8051187598760756181, 0.8051762041353545118, 0.8052336483946334056, 0.8054634254317489805, 0.8063825335802112804, 0.8068420876544424303, 0.8070718646915580052, 0.8071293089508368990, 0.8071580310804763458, 0.8071723921452961248, 0.8071867532101157927, 0.8073016417286735802, 0.8077611958029046191, 0.8079909728400201940, 0.8081058613585779815, 0.8081633056178567642, 0.8081920277474962111, 0.8082207498771356580, 0.8091398580255978468, 0.8091973022848767405, 0.8092116633496964084, 0.8092260244145160764, 0.8092547465441555232, 0.8093696350627133107, 0.8095994120998287746, 0.8100589661740598135, 0.8109780743225218913, 0.8112078513596373552, 0.8112365734892768021, 0.8112652956189162490, 0.8113227398781951427, 0.8114376283967528192, 0.8118971824709838581, 0.8128162906194458248, 0.8130460676565613998, 0.8131609561751190762, 0.8132184004343979700, 0.8132471225640374168, 0.8132614836288570848, 0.8132758446936768637, 0.8137353987679079026, 0.8146545069163698694, 0.8151140609906009082, 0.8152289495091586957, 0.8152863937684375895, 0.8153151158980770363, 0.8153438380277164832, 0.8155736150648319471, 0.8164927232132941359, 0.8169522772875251748, 0.8171820543246406388, 0.8172969428431984262, 0.8173256649728378731, 0.8173328455052477626, 0.8173364357714526518, 0.8173400260376576520, 0.8173543871024773200, 0.8174118313617562137, 0.8192500476586801472, 0.8193074919179590410, 0.8193362140475984878, 0.8193505751124181558, 0.8193649361772379347, 0.8194798246957956112, 0.8197096017329110751, 0.8201691558071420030, 0.8210882639556038587, 0.8213180409927193226, 0.8213754852519982164, 0.8214042073816376632, 0.8214329295112771101, 0.8215478180298347866, 0.8220073721040658254, 0.8229264802525277922, 0.8233860343267587201, 0.8238455884009896479, 0.8247646965494516147, 0.8252242506236825426, 0.8253391391422403300, 0.8253965834015192238, 0.8254253055311586706, 0.8254540276607981175, 0.8256838046979135814, 0.8266029128463754372, 0.8270624669206063651, 0.8272922439577218290, 0.8274071324762795054, 0.8274645767355583992, 0.8275220209948372929, 0.8284411291432991487 ),
 .UNSPECIFIED. ) ;
#14020 = CARTESIAN_POINT ( 'NONE',  ( 0.000000000000000000, 80.93000000000000682, -13.50000000000000000 ) ) ;
#14021 = CARTESIAN_POINT ( 'NONE',  ( -3.636496289402152637, -5.669999999999994600, -11.19198476289190936 ) ) ;
#14022 = CARTESIAN_POINT ( 'NONE',  ( 12.58706070538537425, 69.25271909279739191, 4.887953961977841821 ) ) ;
#14023 = CARTESIAN_POINT ( 'NONE',  ( -2.902129482468654764, 37.28434955807667706, -13.18442075298268712 ) ) ;
#14024 = CARTESIAN_POINT ( 'NONE',  ( 19.29752010712840615, 5.918584287042170544, 17.42428528562864898 ) ) ;
#14025 = CARTESIAN_POINT ( 'NONE',  ( -7.714727599197334307, -62.40312499999986073, -18.62500000000064659 ) ) ;
#14026 = CARTESIAN_POINT ( 'NONE',  ( -10.58212249187060472, 73.61066026166233200, -8.382645537578081729 ) ) ;
#14027 = CARTESIAN_POINT ( 'NONE',  ( -9.417897376538508780, 76.54953983149943042, -9.672290812086593803 ) ) ;
#14028 = CARTESIAN_POINT ( 'NONE',  ( -1.297534681090767750, 7.924607901204613114, -18.46823281779982295 ) ) ;
#14029 = DIRECTION ( 'NONE',  ( -0.000000000000000000, 1.000000000000000000, -0.000000000000000000 ) ) ;
#14030 = CARTESIAN_POINT ( 'NONE',  ( -11.52888015854885317, 80.93000000000003524, -3.329402692648984363 ) ) ;
#14031 = CARTESIAN_POINT ( 'NONE',  ( -8.343458848123576743, 29.48000000000000753, -11.48378591275254301 ) ) ;
#14032 = CARTESIAN_POINT ( 'NONE',  ( 9.520470885617717371, -9.269999999999999574, -6.917026985038131848 ) ) ;
#14033 = CARTESIAN_POINT ( 'NONE',  ( 11.76794919243112325, 40.27999999999998693, 3.823638476888997051 ) ) ;
#14034 = UNCERTAINTY_MEASURE_WITH_UNIT (LENGTH_MEASURE( 1.000000000000000082E-05 ), #8623, 'distance_accuracy_value', 'NONE');
#14035 = CARTESIAN_POINT ( 'NONE',  ( 19.29752010712840615, 0.000000000000000000, 17.42428528562864898 ) ) ;
#14036 = CARTESIAN_POINT ( 'NONE',  ( -1.388145184345592753, 32.63015141958924659, 13.42855714285366631 ) ) ;
#14037 = CARTESIAN_POINT ( 'NONE',  ( 8.213066728255030924, 74.99246367489935494, 10.71458833715021797 ) ) ;
#14038 = CARTESIAN_POINT ( 'NONE',  ( 10.92172942406178926, 3.129999999999993676, 7.935100905948385908 ) ) ;
#14039 =( NAMED_UNIT ( * ) SI_UNIT ( $, .STERADIAN. ) SOLID_ANGLE_UNIT ( ) );
#14040 = CARTESIAN_POINT ( 'NONE',  ( -4.171729424061791036, 82.53000000000000114, 12.83926296998457239 ) ) ;
#14041 = CARTESIAN_POINT ( 'NONE',  ( -2.600835754285047319, 58.27351591942388609, -13.24722694462289141 ) ) ;
#14042 = CARTESIAN_POINT ( 'NONE',  ( -6.944664154335186801, 38.42265581552923237, 11.57681684740535388 ) ) ;
#14043 = CARTESIAN_POINT ( 'NONE',  ( 5.734972866248251755, 36.97144598669994764, -12.22129836149683513 ) ) ;
#14044 = CYLINDRICAL_SURFACE ( 'NONE', #13900, 13.50000000000000000 ) ;
#14045 = LINE ( 'NONE', #6122, #1025 ) ;
#14046 = CARTESIAN_POINT ( 'NONE',  ( 7.037443801358370443, 62.94122972340164779, 11.52066418650788293 ) ) ;
#14047 = CARTESIAN_POINT ( 'NONE',  ( 8.302061766585694613, 41.99651312526439284, 10.64547685796597420 ) ) ;
#14048 = CARTESIAN_POINT ( 'NONE',  ( 7.849181362486006286, 48.88379379287454896, -10.98497563233463659 ) ) ;
#14049 = CARTESIAN_POINT ( 'NONE',  ( 11.76794919243112680, 17.57999999999999829, -3.823638476888993942 ) ) ;
#14050 = ADVANCED_FACE ( 'NONE', ( #13463 ), #7836, .F. ) ;
#14051 = ORIENTED_EDGE ( 'NONE', *, *, #16787, .T. ) ;
#14052 = CARTESIAN_POINT ( 'NONE',  ( 9.520470885617717371, 64.72999999999998977, -6.917026985038131848 ) ) ;
#14053 = CARTESIAN_POINT ( 'NONE',  ( 13.16986379959833897, -90.56874999999976694, 13.16986379960055409 ) ) ;
#14054 = CARTESIAN_POINT ( 'NONE',  ( 4.711679271994910323, -36.42187499999990763, -11.37499999999960387 ) ) ;
#14055 = CARTESIAN_POINT ( 'NONE',  ( -10.92172942406178926, 4.629999999999995453, -7.935100905948389460 ) ) ;
#14056 = CARTESIAN_POINT ( 'NONE',  ( 11.76794919243112680, 32.58000000000001251, -3.823638476888993942 ) ) ;
#14057 = CARTESIAN_POINT ( 'NONE',  ( 0.8559505999959272637, 76.14922317426433551, -13.47283824510951611 ) ) ;
#14058 = AXIS2_PLACEMENT_3D ( 'NONE', #10320, #12960, #7495 ) ;
#14059 = CARTESIAN_POINT ( 'NONE',  ( 10.92172942406179104, 4.730000000000011973, -7.935100905948385908 ) ) ;
#14060 = CARTESIAN_POINT ( 'NONE',  ( 7.714727599200458030, -53.07187499999987068, -18.62499999999935341 ) ) ;
#14061 = CARTESIAN_POINT ( 'NONE',  ( 6.923942340376762594, 65.93627631632044483, 11.60134431817299117 ) ) ;
#14062 = CARTESIAN_POINT ( 'NONE',  ( 10.92172942406178926, 81.13000000000000966, 7.935100905948387684 ) ) ;
#14063 = CARTESIAN_POINT ( 'NONE',  ( -3.636496289402155746, 54.52999999999999403, 11.19198476289190936 ) ) ;
#14064 = CARTESIAN_POINT ( 'NONE',  ( 2.272985001014427788E-15, 59.17999999999998550, -12.37355403259654985 ) ) ;
#14065 = CARTESIAN_POINT ( 'NONE',  ( -9.810502609816827757, 46.56925146285257000, -9.274434226274468784 ) ) ;
#14066 = CARTESIAN_POINT ( 'NONE',  ( 10.93984686930985895, 45.72887148577164851, -7.911647713641231761 ) ) ;
#14067 = CARTESIAN_POINT ( 'NONE',  ( 0.07395759035408112914, 70.17734075790797021, -13.50000000181907467 ) ) ;
#14068 =( NAMED_UNIT ( * ) SI_UNIT ( $, .STERADIAN. ) SOLID_ANGLE_UNIT ( ) );
#14069 = CARTESIAN_POINT ( 'NONE',  ( 4.677241269952973290, 31.01107242823733046, -12.66918181086320061 ) ) ;
#14070 = CARTESIAN_POINT ( 'NONE',  ( -12.79867627401926100, 56.08469950320211694, 4.295844407513158991 ) ) ;
#14071 = CARTESIAN_POINT ( 'NONE',  ( -0.4447223339203151826, 50.66423004611947789, 13.50000000035602099 ) ) ;
#14072 = CARTESIAN_POINT ( 'NONE',  ( 13.04807147248227395, 33.30564593050542754, 3.492245395005759701 ) ) ;
#14073 = CARTESIAN_POINT ( 'NONE',  ( 5.221946460518151589, 42.99121459397418477, -12.44964204775182814 ) ) ;
#14074 = CARTESIAN_POINT ( 'NONE',  ( 7.736074338173390963, 39.88885195608636991, -11.06766002516535607 ) ) ;
#14075 = ORIENTED_EDGE ( 'NONE', *, *, #10937, .F. ) ;
#14076 = CARTESIAN_POINT ( 'NONE',  ( -13.07942562849002499, 61.81060098926703716, -3.356404025825254767 ) ) ;
#14077 = ORIENTED_EDGE ( 'NONE', *, *, #8816, .T. ) ;
#14078 = CARTESIAN_POINT ( 'NONE',  ( -5.491332954668864730, -19.60957387106639516, 16.75890910139807843 ) ) ;
#14079 = CARTESIAN_POINT ( 'NONE',  ( 18.62500000000064304, -34.34062499999991047, -7.714727599197335195 ) ) ;
#14080 = CARTESIAN_POINT ( 'NONE',  ( 4.748822866441054558, 58.00894215750955141, -12.63719586234929437 ) ) ;
#14081 = VECTOR ( 'NONE', #9253, 1000.000000000000000 ) ;
#14082 = CARTESIAN_POINT ( 'NONE',  ( 9.520470885617715595, 76.13000000000000966, 6.917026985038134512 ) ) ;
#14083 = CARTESIAN_POINT ( 'NONE',  ( 11.68790604918427789, -2.350847233825327770E-15, -4.414367548897630833 ) ) ;
#14084 = B_SPLINE_CURVE_WITH_KNOTS ( 'NONE', 3,
 ( #11090, #5792, #4097, #8184, #13545, #12231, #387, #1701, #13717, #11177 ),
 .UNSPECIFIED., .F., .F.,
 ( 4, 2, 2, 2, 4 ),
 ( 0.002109865028651171977, 0.002636639667304636111, 0.003163414305958100244, 0.003690188944611564378, 0.004216963583265028945 ),
 .UNSPECIFIED. ) ;
#14085 = CARTESIAN_POINT ( 'NONE',  ( -9.581374244281432695, 46.55771639631056047, -9.510429861097501103 ) ) ;
#14086 = DIRECTION ( 'NONE',  ( 0.000000000000000000, 0.000000000000000000, 1.000000000000000000 ) ) ;
#14087 = CARTESIAN_POINT ( 'NONE',  ( 8.043339635996302306, -7.318749999999964118, 8.043339635997654113 ) ) ;
#14088 = CARTESIAN_POINT ( 'NONE',  ( 10.68047679364148372, 54.11617973143395943, 8.256962218962808464 ) ) ;
#14089 = AXIS2_PLACEMENT_3D ( 'NONE', #8081, #6838, #1601 ) ;
#14090 = ORIENTED_EDGE ( 'NONE', *, *, #595, .T. ) ;
#14091 = FACE_OUTER_BOUND ( 'NONE', #15061, .T. ) ;
#14092 = EDGE_CURVE ( 'NONE', #546, #14477, #15846, .T. ) ;
#14093 = ORIENTED_EDGE ( 'NONE', *, *, #4067, .F. ) ;
#14094 = CARTESIAN_POINT ( 'NONE',  ( 10.92172942406178926, 9.129999999999999005, 7.935100905948385908 ) ) ;
#14095 = CARTESIAN_POINT ( 'NONE',  ( -3.037551701948927096, 34.28921878658023559, -13.15470998141922365 ) ) ;
#14096 = CARTESIAN_POINT ( 'NONE',  ( 8.043339635996300530, -97.81874999999976694, 8.043339635997654113 ) ) ;
#14097 = CARTESIAN_POINT ( 'NONE',  ( 5.572222782050855194, 77.88196720139393392, 12.30424787591440783 ) ) ;
#14098 = CARTESIAN_POINT ( 'NONE',  ( 10.92172942406179104, 47.73000000000000398, -7.935100905948385908 ) ) ;
#14099 = CARTESIAN_POINT ( 'NONE',  ( 16.64312382832869730, 7.924527542031523097, 8.110285629053034739 ) ) ;
#14100 = DIRECTION ( 'NONE',  ( -0.000000000000000000, 1.000000000000000000, -0.000000000000000000 ) ) ;
#14101 = CARTESIAN_POINT ( 'NONE',  ( 12.90825826996955250, 72.28807910334995768, 3.957424788451787467 ) ) ;
#14102 = CARTESIAN_POINT ( 'NONE',  ( 2.279995255611139653E-15, 27.18000000000000682, -12.37355403259654985 ) ) ;
#14103 = CARTESIAN_POINT ( 'NONE',  ( 8.343458848123578520, 62.97999999999999687, 11.48378591275254124 ) ) ;
#14104 = CARTESIAN_POINT ( 'NONE',  ( -3.536773975472625509, 52.30716712712094107, -13.03489925632436908 ) ) ;
#14105 = B_SPLINE_CURVE_WITH_KNOTS ( 'NONE', 3,
 ( #150, #5556, #10940, #13656, #15059, #4391, #5732, #1639, #1726, #9801, #15147, #3045, #13826, #1809, #839, #17015, #7578, #3495 ),
 .UNSPECIFIED., .F., .F.,
 ( 4, 2, 2, 2, 2, 2, 2, 2, 4 ),
 ( 2.344180274388505431E-07, 0.0005273255548235199555, 0.001054416691619601077, 0.001581507828415682198, 0.002108598965211763536, 0.002635690102007839236, 0.003162781238803915370, 0.003689872375599991070, 0.004216963512396067204 ),
 .UNSPECIFIED. ) ;
#14106 = CARTESIAN_POINT ( 'NONE',  ( 11.76794919243112680, 40.57999999999999829, -3.823638476888993942 ) ) ;
#14107 = CARTESIAN_POINT ( 'NONE',  ( 7.272992578804311492, -15.12000000000000277, -10.01041549318726709 ) ) ;
#14108 = CARTESIAN_POINT ( 'NONE',  ( -13.49999999999999822, 54.77999999999998693, -4.386415899144240349 ) ) ;
#14109 = LINE ( 'NONE', #14020, #242 ) ;
#14110 = CARTESIAN_POINT ( 'NONE',  ( 3.236805660951904251, 68.79646791454764809, 13.10715617363204544 ) ) ;
#14111 = CARTESIAN_POINT ( 'NONE',  ( 18.62499999999934630, -32.25937499999992042, 7.714727599200467800 ) ) ;
#14112 = CARTESIAN_POINT ( 'NONE',  ( -4.171729424061787483, 4.330000000000000071, -12.83926296998457417 ) ) ;
#14113 = CARTESIAN_POINT ( 'NONE',  ( -13.16986379959834252, -96.74374999999980673, -13.16986379960055409 ) ) ;
#14114 = CARTESIAN_POINT ( 'NONE',  ( -13.48413585140022519, 73.95268284379521617, 0.6581954568009130702 ) ) ;
#14115 = CARTESIAN_POINT ( 'NONE',  ( -9.416305305992766606, 76.54946069877891546, -9.673840839019193893 ) ) ;
#14116 = LINE ( 'NONE', #4765, #5936 ) ;
#14117 = CARTESIAN_POINT ( 'NONE',  ( 9.110082863707074097, 8.062255781930765863, -15.52458835467165699 ) ) ;
#14118 = CARTESIAN_POINT ( 'NONE',  ( 7.272992578804311492, 34.87999999999999545, -10.01041549318726886 ) ) ;
#14119 = CARTESIAN_POINT ( 'NONE',  ( 6.767892274116773521, 80.93000000001259764, -11.68099457092376348 ) ) ;
#14120 = CARTESIAN_POINT ( 'NONE',  ( -6.462491681254555864, 32.44254954019859127, 11.85507982337297150 ) ) ;
#14121 = CARTESIAN_POINT ( 'NONE',  ( -19.79706521687757359, 7.170682760640493925, -8.000000000000232703 ) ) ;
#14122 = CARTESIAN_POINT ( 'NONE',  ( 11.37500000000007816, 4.439344646909156023E-16, -0.9008532055000779692 ) ) ;
#14123 = B_SPLINE_CURVE_WITH_KNOTS ( 'NONE', 3,
 ( #15414, #7312, #11549, #12785, #6250, #10233, #4656, #10317, #14265, #11463, #4829, #584, #16839, #15498, #5995, #4919, #11377, #2154, #3410, #3137, #12872, #8562, #16749, #8824, #10064, #3320, #14182, #2067, #7491, #761, #3329, #14446, #9093, #16757, #6002, #1986, #16848, #3418, #8832, #14189, #1024, #15944, #1109, #11904, #10906, #6435, #11819, #13710, #14529, #9593, #2415, #17198, #7933, #17281, #10498, #10995, #4358, #15113, #5195, #6936, #5106, #6525, #13137, #12224, #15861, #9267, #10583, #6846, #16456, #3768, #14944, #9180, #7848, #1429, #13307, #7766, #208, #1519, #5522, #8266, #13221, #16275, #12314, #3852, #14618, #2504, #116, #4181, #9767, #2835, #13627, #5613, #7026, #16363, #4270, #292, #9680, #15030, #2923, #8353, #1609, #12404, #5701, #11082, #11254, #15205, #15465, #16545, #635, #10030, #16633, #8532, #3105, #467, #2033, #5875, #1781, #12840, #15292, #4536, #16801, #13796, #7190, #7109, #3375, #5960, #379, #550, #13880, #1946, #15377, #13967, #7368, #1694, #1864, #726, #6135, #12493, #11170, #5785, #4451, #9858, #7278, #3284, #12661, #12579, #8700, #14145, #4796, #9944, #14061, #7458, #3194, #10112, #6048, #8615, #11340, #16717, #4623, #12748, #11431, #16891, #4709, #11514, #10197, #3011, #8441, #13180, #8876, #2202, #3631, #2115, #9137, #15634, #1065, #9045, #5060, #14397, #5149, #7628, #7714, #14576, #13266, #5237, #1154, #15550, #4647, #14172, #829, #11368 ),
 .UNSPECIFIED., .F., .F.,
 ( 4, 2, 2, 2, 2, 1, 1, 2, 2, 1, 1, 2, 2, 1, 1, 2, 2, 2, 2, 2, 2, 1, 2, 2, 2, 2, 1, 2, 2, 1, 2, 2, 2, 2, 2, 1, 1, 2, 2, 2, 2, 2, 2, 1, 2, 2, 2, 2, 1, 2, 2, 1, 1, 2, 1, 1, 1, 2, 2, 2, 2, 2, 2, 2, 1, 1, 2, 2, 2, 1, 2, 2, 1, 1, 1, 2, 2, 1, 2, 2, 1, 2, 2, 2, 2, 1, 2, 2, 2, 2, 2, 2, 2, 1, 1, 1, 2, 2, 2, 1, 1, 2, 2, 1, 2, 2, 2, 2, 2, 2, 1, 4 ),
 ( 0.2696254849433896150, 0.2705427676827099059, 0.2714600504220301413, 0.2715173805932376561, 0.2715747107644451708, 0.2716893711068602002, 0.2719186917916902591, 0.2723773331613503768, 0.2732946159006706122, 0.2734092762430856416, 0.2734236087858875064, 0.2734307750572884665, 0.2734379413286894267, 0.2734666064142931563, 0.2735239365855006710, 0.2737532572703307299, 0.2742118986399908476, 0.2751291813793110275, 0.2753585020641410863, 0.2753871671497448159, 0.2754158322353486010, 0.2754731624065561157, 0.2755878227489711452, 0.2760464641186312629, 0.2769637468579514983, 0.2771930675427815571, 0.2773077278851965866, 0.2773363929708003717, 0.2773650580564041013, 0.2774223882276116160, 0.2778810295972717892, 0.2787983123365920801, 0.2792569537062522533, 0.2792856187918559829, 0.2792999513346579032, 0.2793142838774597680, 0.2793716140486672828, 0.2794862743910823122, 0.2797155950759123710, 0.2806328778152326620, 0.2810915191848927797, 0.2812061795273078091, 0.2812635096985153238, 0.2813208398697228385, 0.2815501605545528974, 0.2824674432938731883, 0.2829260846635333060, 0.2831554053483633648, 0.2831840704339671499, 0.2831984029767690147, 0.2832127355195708795, 0.2832700656907784498, 0.2833847260331934792, 0.2843020087725137701, 0.2847606501421739433, 0.2849899708270040022, 0.2851046311694190871, 0.2851332962550228167, 0.2851619613406266018, 0.2852192915118341165, 0.2861365742511544075, 0.2870538569904746984, 0.2870825220760784280, 0.2871111871616822131, 0.2871685173328897278, 0.2872831776753047572, 0.2875124983601348716, 0.2879711397297950448, 0.2888884224691154468, 0.2890030828115304762, 0.2890604129827380464, 0.2890747455255399112, 0.2890890780683417760, 0.2891177431539455611, 0.2893470638387756200, 0.2898057052084357932, 0.2907229879477561396, 0.2909523086325861985, 0.2910096388037937132, 0.2910383038893974983, 0.2910669689750012279, 0.2911816293174162573, 0.2916402706870764305, 0.2925575534263967770, 0.2927868741112268913, 0.2929015344536419208, 0.2929588646248494355, 0.2930161947960569502, 0.2934748361657171234, 0.2943921189050374698, 0.2948507602746976430, 0.2949080904459051578, 0.2949224229887070781, 0.2949367555315089429, 0.2949654206171127280, 0.2950800809595277574, 0.2953094016443579273, 0.2962266843836784957, 0.2966853257533387800, 0.2967999860957538649, 0.2968573162669613796, 0.2968716488097632444, 0.2968859813525651647, 0.2969146464381688943, 0.2971439671229990087, 0.2980612498623194107, 0.2985198912319795839, 0.2987492119168096427, 0.2988065420880171574, 0.2988352071736209425, 0.2988638722592247277, 0.2989785326016397571 ),
 .UNSPECIFIED. ) ;
#14124 =( NAMED_UNIT ( * ) PLANE_ANGLE_UNIT ( ) SI_UNIT ( $, .RADIAN. ) );
#14125 = CARTESIAN_POINT ( 'NONE',  ( 13.50000000000000355, 80.57999999999998408, -4.386415899144233244 ) ) ;
#14126 = CARTESIAN_POINT ( 'NONE',  ( 13.19208277413943975, 51.53150884716730218, -2.867894163931984597 ) ) ;
#14127 = FACE_OUTER_BOUND ( 'NONE', #7822, .T. ) ;
#14128 = CARTESIAN_POINT ( 'NONE',  ( 2.196276064027457675, 37.10127726452279262, -13.32743759420177554 ) ) ;
#14129 = CARTESIAN_POINT ( 'NONE',  ( 11.37500000000000000, -66.59999999999983800, 9.531744055041752924E-13 ) ) ;
#14130 = DIRECTION ( 'NONE',  ( 0.000000000000000000, 1.000000000000000000, 0.000000000000000000 ) ) ;
#14131 = CARTESIAN_POINT ( 'NONE',  ( -4.068989761728259325, 49.32630495305625118, -12.87242965585119236 ) ) ;
#14132 = EDGE_CURVE ( 'NONE', #13554, #6499, #71, .T. ) ;
#14133 = CARTESIAN_POINT ( 'NONE',  ( -13.50000000000000000, 60.92999999999999972, -3.306546357697853733E-15 ) ) ;
#14134 = DIRECTION ( 'NONE',  ( 0.000000000000000000, 0.000000000000000000, -1.000000000000000000 ) ) ;
#14135 = CARTESIAN_POINT ( 'NONE',  ( 13.36456123615529634, 48.49836822103661405, -1.955719740300823961 ) ) ;
#14136 = CARTESIAN_POINT ( 'NONE',  ( -11.76794919243112325, 21.77999999999999758, -3.823638476888998827 ) ) ;
#14137 = ORIENTED_EDGE ( 'NONE', *, *, #9438, .F. ) ;
#14138 = CARTESIAN_POINT ( 'NONE',  ( 3.636496289402154414, 66.82999999999999829, 11.19198476289190936 ) ) ;
#14139 = CARTESIAN_POINT ( 'NONE',  ( -18.62500000000064659, -85.36562499999978115, 7.714727599197333419 ) ) ;
#14140 = CARTESIAN_POINT ( 'NONE',  ( -9.552639591052204498E-13, -45.78749999999988773, 11.37500000000000000 ) ) ;
#14141 = CARTESIAN_POINT ( 'NONE',  ( -4.171729424061791036, 2.530000000000004690, 12.83926296998457239 ) ) ;
#14142 = CARTESIAN_POINT ( 'NONE',  ( 9.520470885617715595, 32.13000000000001677, 6.917026985038135400 ) ) ;
#14143 = CARTESIAN_POINT ( 'NONE',  ( -10.98210873309851898, 80.92999999999996419, -5.183560256216895645 ) ) ;
#14144 = CARTESIAN_POINT ( 'NONE',  ( -18.62500000000064659, -75.96562499999981810, 7.714727599197333419 ) ) ;
#14145 = CARTESIAN_POINT ( 'NONE',  ( 8.105864574935058187, 65.98763176480156289, 10.79566791222186772 ) ) ;
#14146 = DIRECTION ( 'NONE',  ( -0.000000000000000000, -1.000000000000000000, -0.000000000000000000 ) ) ;
#14147 = CARTESIAN_POINT ( 'NONE',  ( -7.272992578804310604, 54.37999999999999545, 10.01041549318726709 ) ) ;
#14148 = CARTESIAN_POINT ( 'NONE',  ( -10.54451491581842504, 59.25158502488826429, 8.432595136247059031 ) ) ;
#14149 = EDGE_CURVE ( 'NONE', #10231, #5098, #4366, .T. ) ;
#14150 = CARTESIAN_POINT ( 'NONE',  ( 9.162143948892088829, 45.82302722542944906, -9.914896862951890100 ) ) ;
#14151 = CARTESIAN_POINT ( 'NONE',  ( 0.7729741899047672948, 70.15223374091664255, -13.48100388766008528 ) ) ;
#14152 = AXIS2_PLACEMENT_3D ( 'NONE', #2, #1064, #14660 ) ;
#14153 = CARTESIAN_POINT ( 'NONE',  ( -9.708203932499367639, 6.763974596215558854, -7.053423027509681198 ) ) ;
#14154 = CARTESIAN_POINT ( 'NONE',  ( 12.01961491643047175, 30.65663574407087921, -6.146451131573384075 ) ) ;
#14155 = CARTESIAN_POINT ( 'NONE',  ( -13.47178327623467631, 55.96039367275813703, 0.8796395391391890195 ) ) ;
#14156 = CARTESIAN_POINT ( 'NONE',  ( 0.000000000000000000, 102.9300000000000068, 0.000000000000000000 ) ) ;
#14157 = CARTESIAN_POINT ( 'NONE',  ( 3.198877721759256776, 32.79499661759405882, 13.12308681134866362 ) ) ;
#14158 = DIRECTION ( 'NONE',  ( 0.5000000000000035527, 0.000000000000000000, -0.8660254037844365982 ) ) ;
#14159 = CARTESIAN_POINT ( 'NONE',  ( 10.29006543620832126, 39.76535928357677108, -8.738724199765389500 ) ) ;
#14160 = VERTEX_POINT ( 'NONE', #7201 ) ;
#14161 = CARTESIAN_POINT ( 'NONE',  ( -8.733024514805581617, 62.34354256471783629, 10.29493024108846733 ) ) ;
#14162 = ORIENTED_EDGE ( 'NONE', *, *, #1462, .F. ) ;
#14163 = ORIENTED_EDGE ( 'NONE', *, *, #8201, .T. ) ;
#14164 = CARTESIAN_POINT ( 'NONE',  ( 8.343458848123583849, 33.87999999999999545, -11.48378591275253768 ) ) ;
#14165 = CARTESIAN_POINT ( 'NONE',  ( -7.714727599197335195, -21.85312499999995239, -18.62500000000064304 ) ) ;
#14166 = CARTESIAN_POINT ( 'NONE',  ( 8.869080463320887731, 48.02207153075600843, 10.21686289651330881 ) ) ;
#14167 = AXIS2_PLACEMENT_3D ( 'NONE', #8728, #920, #14086 ) ;
#14168 = CARTESIAN_POINT ( 'NONE',  ( 4.680006372702086637, 58.01148812036320379, -12.66286395962633726 ) ) ;
#14169 = CARTESIAN_POINT ( 'NONE',  ( 2.537983195068045816, 79.08874347684349004, -13.25928836460632354 ) ) ;
#14170 = CARTESIAN_POINT ( 'NONE',  ( 7.272992578804308828, 81.97999999999998977, 10.01041549318726709 ) ) ;
#14171 = CARTESIAN_POINT ( 'NONE',  ( -10.92172942406178926, 42.63000000000000256, -7.935100905948389460 ) ) ;
#14172 = CARTESIAN_POINT ( 'NONE',  ( 0.1711164140752765850, 65.68615328522727737, 13.49921302317839533 ) ) ;
#14173 = EDGE_CURVE ( 'NONE', #7488, #12569, #16372, .T. ) ;
#14174 =( LENGTH_UNIT ( ) NAMED_UNIT ( * ) SI_UNIT ( .MILLI., .METRE. ) );
#14175 = FACE_OUTER_BOUND ( 'NONE', #13698, .T. ) ;
#14176 = CARTESIAN_POINT ( 'NONE',  ( -11.37500000000000178, -17.72499999999994102, -9.545674412382054647E-13 ) ) ;
#14177 = VECTOR ( 'NONE', #7355, 1000.000000000000000 ) ;
#14178 = CARTESIAN_POINT ( 'NONE',  ( 3.558926121134557530, 53.80781110109241894, 13.02324908181068963 ) ) ;
#14179 = ORIENTED_EDGE ( 'NONE', *, *, #3751, .T. ) ;
#14180 = CARTESIAN_POINT ( 'NONE',  ( 8.378360550312208943, 10.00007452681958497, 10.58551248116806498 ) ) ;
#14181 = VERTEX_POINT ( 'NONE', #10889 ) ;
#14182 = CARTESIAN_POINT ( 'NONE',  ( 5.783146345639755381, 66.96971615883565221, -12.20007971092912413 ) ) ;
#14183 = CARTESIAN_POINT ( 'NONE',  ( 11.37499999999999645, -7.250000000000000000, 9.531744055041752924E-13 ) ) ;
#14184 = DIRECTION ( 'NONE',  ( -0.000000000000000000, 1.000000000000000000, -0.000000000000000000 ) ) ;
#14185 = DIRECTION ( 'NONE',  ( 0.000000000000000000, -1.000000000000000000, 0.000000000000000000 ) ) ;
#14186 = CARTESIAN_POINT ( 'NONE',  ( 15.43494339453338426, 7.854708401161940579, 10.68872673103595794 ) ) ;
#14187 = CARTESIAN_POINT ( 'NONE',  ( -8.343458848123582072, 6.380000000000007887, 11.48378591275253768 ) ) ;
#14188 = CARTESIAN_POINT ( 'NONE',  ( 13.38186479756907232, 72.36768824479015905, 1.782328871136838133 ) ) ;
#14189 = CARTESIAN_POINT ( 'NONE',  ( 8.546315828672829795, 66.85235120296643174, -10.45335113635833757 ) ) ;
#14190 = CARTESIAN_POINT ( 'NONE',  ( -7.409984580736203970E-16, 28.67999999999999972, 12.37355403259654985 ) ) ;
#14191 = CARTESIAN_POINT ( 'NONE',  ( -8.343458848123576743, 49.47999999999998977, -11.48378591275254301 ) ) ;
#14192 = CARTESIAN_POINT ( 'NONE',  ( -0.2119980460951424450, 71.67237679919810489, 13.49880501296570579 ) ) ;
#14193 = VECTOR ( 'NONE', #5651, 1000.000000000000000 ) ;
#14194 = EDGE_CURVE ( 'NONE', #3134, #2050, #805, .T. ) ;
#14195 = CARTESIAN_POINT ( 'NONE',  ( -8.343458848123576743, 51.47999999999998977, -11.48378591275254301 ) ) ;
#14196 = CARTESIAN_POINT ( 'NONE',  ( 18.02297152527631141, 8.055324227812098670, 0.3502263562676400377 ) ) ;
#14197 = CARTESIAN_POINT ( 'NONE',  ( -6.636343628379751003, 68.43540020522837608, 11.76870444476310773 ) ) ;
#14198 = CARTESIAN_POINT ( 'NONE',  ( 7.714727599200458030, -19.77187499999995168, -18.62499999999934985 ) ) ;
#14199 = CARTESIAN_POINT ( 'NONE',  ( 4.171729424061789260, 70.82999999999999829, 12.83926296998457417 ) ) ;
#14200 = CARTESIAN_POINT ( 'NONE',  ( 18.62499999999934630, -48.90937499999989058, 7.714727599200467800 ) ) ;
#14201 = CARTESIAN_POINT ( 'NONE',  ( -2.434037520544789945, 65.59248196249376406, 13.27883458231978331 ) ) ;
#14202 = CARTESIAN_POINT ( 'NONE',  ( 0.000000000000000000, 80.93000000000000682, 0.000000000000000000 ) ) ;
#14203 = CARTESIAN_POINT ( 'NONE',  ( -2.138189944381320373, 2.256881422320268893, -13.49999999999997335 ) ) ;
#14204 = CARTESIAN_POINT ( 'NONE',  ( 13.49999999999999822, 50.28000000000000114, 4.386415899144236796 ) ) ;
#14205 = CARTESIAN_POINT ( 'NONE',  ( 0.000000000000000000, 9.000000000000000000, -14.50000000000000000 ) ) ;
#14206 = CARTESIAN_POINT ( 'NONE',  ( -13.22310757530384784, 31.83334110198622469, -2.736780972190429928 ) ) ;
#14207 = CARTESIAN_POINT ( 'NONE',  ( 5.908864746862505513, 74.89534936253288322, 12.13818304319435448 ) ) ;
#14208 = LINE ( 'NONE', #4858, #6278 ) ;
#14209 = CARTESIAN_POINT ( 'NONE',  ( -10.92172942406178926, 72.62999999999999545, -7.935100905948389460 ) ) ;
#14210 = ADVANCED_FACE ( 'NONE', ( #13612 ), #16165, .F. ) ;
#14211 = CARTESIAN_POINT ( 'NONE',  ( 13.23613990012235142, 51.52375947025169012, -2.656052883722033631 ) ) ;
#14212 = CARTESIAN_POINT ( 'NONE',  ( -9.433473205167290487, 38.30967010535225370, 9.657148195847520711 ) ) ;
#14213 = CARTESIAN_POINT ( 'NONE',  ( 11.39132066586519265, 36.70125830944373035, -7.245326858912307877 ) ) ;
#14214 = CARTESIAN_POINT ( 'NONE',  ( -11.37500000000039613, -33.26562499999994316, 4.711679271993000739 ) ) ;
#14215 = DIRECTION ( 'NONE',  ( 0.8660254037844413721, 0.000000000000000000, -0.4999999999999953926 ) ) ;
#14216 = CARTESIAN_POINT ( 'NONE',  ( -6.438066478122774328, 77.44350536356481030, 11.86602938538363894 ) ) ;
#14217 = CARTESIAN_POINT ( 'NONE',  ( -2.138189944381219565, 61.60311857767971588, 13.50000000000000355 ) ) ;
#14218 = CARTESIAN_POINT ( 'NONE',  ( 1.241788420113878466, 41.72465377607231574, 13.44682026920488127 ) ) ;
#14219 = CARTESIAN_POINT ( 'NONE',  ( 12.24640860966871969, 48.63820562460364272, -5.681204235008639358 ) ) ;
#14220 = CARTESIAN_POINT ( 'NONE',  ( 9.520470885617717371, 11.73000000000000398, -6.917026985038131848 ) ) ;
#14221 = CYLINDRICAL_SURFACE ( 'NONE', #10902, 13.50000000000000000 ) ;
#14222 = ORIENTED_EDGE ( 'NONE', *, *, #9898, .F. ) ;
#14223 = CARTESIAN_POINT ( 'NONE',  ( -3.636496289402153081, 62.32999999999999829, -11.19198476289190936 ) ) ;
#14224 = CARTESIAN_POINT ( 'NONE',  ( 4.711679271993006957, -6.278124999999967315, 11.37500000000039613 ) ) ;
#14225 = CARTESIAN_POINT ( 'NONE',  ( 12.50000000000000000, -18.00000000000000355, -2.204364238465235822E-15 ) ) ;
#14226 = CARTESIAN_POINT ( 'NONE',  ( -8.343458848123576743, -1.519999999999997131, -11.48378591275254301 ) ) ;
#14227 = CARTESIAN_POINT ( 'NONE',  ( -9.520470885617715595, 30.63000000000001677, -6.917026985038136289 ) ) ;
#14228 = CARTESIAN_POINT ( 'NONE',  ( -5.318689435344804650, 80.93000000000000682, -11.55616787654882671 ) ) ;
#14229 = CARTESIAN_POINT ( 'NONE',  ( -1.564113515457998572E-12, -79.08749999999980673, 18.62500000000000000 ) ) ;
#14230 = VECTOR ( 'NONE', #5627, 1000.000000000000000 ) ;
#14231 = CARTESIAN_POINT ( 'NONE',  ( 1.732050807568875195, 0.000000000000000000, -19.00000000000000000 ) ) ;
#14232 = CARTESIAN_POINT ( 'NONE',  ( -7.272992578804310604, 45.38000000000000256, 10.01041549318726709 ) ) ;
#14233 = EDGE_CURVE ( 'NONE', #1687, #13257, #2645, .T. ) ;
#14234 = CARTESIAN_POINT ( 'NONE',  ( -11.71428983209350072, 59.17987341424922931, 6.726823528539508601 ) ) ;
#14235 = CARTESIAN_POINT ( 'NONE',  ( 13.21512175077752538, 45.33208276352622335, 2.769527569284461421 ) ) ;
#14236 = DIRECTION ( 'NONE',  ( -0.000000000000000000, 1.000000000000000000, -0.000000000000000000 ) ) ;
#14237 = DIRECTION ( 'NONE',  ( 0.000000000000000000, -1.000000000000000000, 0.000000000000000000 ) ) ;
#14238 = CARTESIAN_POINT ( 'NONE',  ( 13.49051628622518173, 30.44740727456623119, -0.5059554888960394736 ) ) ;
#14239 = CARTESIAN_POINT ( 'NONE',  ( -13.48278874607188271, 55.90643395278321748, -0.6820209318931385045 ) ) ;
#14240 = CARTESIAN_POINT ( 'NONE',  ( 17.42428528562844292, 0.000000000000000000, 19.29752010712858024 ) ) ;
#14241 = CARTESIAN_POINT ( 'NONE',  ( 5.367902793731293087, 63.98565814275196573, -12.38691854761588296 ) ) ;
#14242 = CARTESIAN_POINT ( 'NONE',  ( 19.79695994079629529, 7.170708369609773314, -7.999999999999952927 ) ) ;
#14243 = CARTESIAN_POINT ( 'NONE',  ( 13.04481288137828265, 39.55393178331779325, -3.476205045992002418 ) ) ;
#14244 = ORIENTED_EDGE ( 'NONE', *, *, #7558, .T. ) ;
#14245 = CARTESIAN_POINT ( 'NONE',  ( -12.39398694249804400, 61.73475989268117559, -5.356182190199231918 ) ) ;
#14246 = ORIENTED_EDGE ( 'NONE', *, *, #5760, .F. ) ;
#14247 = ORIENTED_EDGE ( 'NONE', *, *, #6336, .F. ) ;
#14248 = CARTESIAN_POINT ( 'NONE',  ( -3.636496289402152637, -17.66999999999999815, -11.19198476289190936 ) ) ;
#14249 = CARTESIAN_POINT ( 'NONE',  ( 18.62500000000000000, -33.29999999999991900, 1.560692158462880521E-12 ) ) ;
#14250 = CARTESIAN_POINT ( 'NONE',  ( 10.74742752807278734, 48.11997365494462997, 8.169672665494852382 ) ) ;
#14251 = CARTESIAN_POINT ( 'NONE',  ( 2.197686288218880346, 58.10098381549926927, -13.32020416656907891 ) ) ;
#14252 = CARTESIAN_POINT ( 'NONE',  ( 8.224420489434695725, 78.86728963787211910, -10.71480034530365621 ) ) ;
#14253 = CARTESIAN_POINT ( 'NONE',  ( -9.520470885617715595, 77.63000000000000966, -6.917026985038136289 ) ) ;
#14254 = CARTESIAN_POINT ( 'NONE',  ( 10.98232607281872397, -2.350847233825325403E-15, -5.687886418642680297 ) ) ;
#14255 = CARTESIAN_POINT ( 'NONE',  ( 2.138189944381158725, 2.103118577679734091, -13.50000000000002487 ) ) ;
#14256 = SURFACE_STYLE_FILL_AREA ( #753 ) ;
#14257 = CARTESIAN_POINT ( 'NONE',  ( 0.000000000000000000, 0.000000000000000000, 5.000000000000000000 ) ) ;
#14258 = CARTESIAN_POINT ( 'NONE',  ( 11.37500000000000178, -9.399999999999959499, 9.531744055041752924E-13 ) ) ;
#14259 = CIRCLE ( 'NONE', #12594, 26.00000000000000355 ) ;
#14260 = CARTESIAN_POINT ( 'NONE',  ( -4.171729424061791036, 79.53000000000000114, 12.83926296998457239 ) ) ;
#14261 = CARTESIAN_POINT ( 'NONE',  ( 8.198328110229137877, 33.86819861533544440, -10.72568410487125412 ) ) ;
#14262 = VERTEX_POINT ( 'NONE', #3088 ) ;
#14263 = DIRECTION ( 'NONE',  ( 0.000000000000000000, 1.000000000000000000, 0.000000000000000000 ) ) ;
#14264 = ORIENTED_EDGE ( 'NONE', *, *, #10622, .F. ) ;
#14265 = CARTESIAN_POINT ( 'NONE',  ( 2.776197549605788240, 67.08017814200591999, -13.21149016882078087 ) ) ;
#14266 = B_SPLINE_CURVE_WITH_KNOTS ( 'NONE', 3,
 ( #3129, #16655, #7216, #12603, #11369, #15491, #664, #7483, #12864, #2400 ),
 .UNSPECIFIED., .F., .F.,
 ( 4, 2, 2, 2, 4 ),
 ( 0.002109865028651037970, 0.002636639667304533328, 0.003163414305958029121, 0.003690188944611524913, 0.004216963583265020271 ),
 .UNSPECIFIED. ) ;
#14267 = CARTESIAN_POINT ( 'NONE',  ( 8.043339635996298753, -38.46874999999992895, 8.043339635997652337 ) ) ;
#14268 = EDGE_CURVE ( 'NONE', #4303, #1772, #3448, .T. ) ;
#14269 = CARTESIAN_POINT ( 'NONE',  ( 0.000000000000000000, 80.93000000000000682, -13.50000000000000000 ) ) ;
#14270 = CARTESIAN_POINT ( 'NONE',  ( -0.7687312486613894214, 59.65236697067454941, 13.47875314867014573 ) ) ;
#14271 = CYLINDRICAL_SURFACE ( 'NONE', #5664, 8.999999999999998224 ) ;
#14272 = PLANE ( 'NONE',  #15876 ) ;
#14273 = CARTESIAN_POINT ( 'NONE',  ( 9.940909119425192841, 72.07613200268791331, 9.134167122504003089 ) ) ;
#14274 = AXIS2_PLACEMENT_3D ( 'NONE', #12205, #11322, #16437 ) ;
#14275 = CARTESIAN_POINT ( 'NONE',  ( -13.50000000000000000, 55.92999999999999972, -3.306546357697853733E-15 ) ) ;
#14276 = CARTESIAN_POINT ( 'NONE',  ( -1.005545769327274827E-13, 52.18000000000000682, -13.50000000000000000 ) ) ;
#14277 = CARTESIAN_POINT ( 'NONE',  ( 8.343458848123580296, 76.98000000000000398, 11.48378591275253768 ) ) ;
#14278 = CARTESIAN_POINT ( 'NONE',  ( 1.561832610794586538E-12, -70.76249999999983231, -18.62500000000000000 ) ) ;
#14279 = CARTESIAN_POINT ( 'NONE',  ( -0.4448446338779524223, 68.66416886155738553, 13.49450202653779307 ) ) ;
#14280 = CARTESIAN_POINT ( 'NONE',  ( -13.16986379960055231, -60.35624999999985363, 13.16986379959834252 ) ) ;
#14281 = DIRECTION ( 'NONE',  ( 0.000000000000000000, 0.000000000000000000, -1.000000000000000000 ) ) ;
#14282 = CARTESIAN_POINT ( 'NONE',  ( -13.16986379959834252, -22.89374999999994387, -13.16986379960055054 ) ) ;
#14283 = AXIS2_PLACEMENT_3D ( 'NONE', #8908, #3407, #2152 ) ;
#14284 = CARTESIAN_POINT ( 'NONE',  ( -2.273536850346836502, 65.59826044952400537, 13.30738196274165297 ) ) ;
#14285 = DIRECTION ( 'NONE',  ( 0.000000000000000000, 0.7071067811865460184, 0.7071067811865490160 ) ) ;
#14286 = CARTESIAN_POINT ( 'NONE',  ( 0.000000000000000000, 80.93000000000000682, 0.000000000000000000 ) ) ;
#14287 = EDGE_CURVE ( 'NONE', #14307, #15397, #9490, .T. ) ;
#14288 = ORIENTED_EDGE ( 'NONE', *, *, #4889, .F. ) ;
#14289 = CARTESIAN_POINT ( 'NONE',  ( 7.312260103668256263E-16, 8.062177826491094379, -18.00000000000000000 ) ) ;
#14290 = CYLINDRICAL_SURFACE ( 'NONE', #9209, 13.50000000000000000 ) ;
#14291 = CARTESIAN_POINT ( 'NONE',  ( -12.60192476712481557, 32.10554672858959435, 4.841671032898100080 ) ) ;
#14292 = CARTESIAN_POINT ( 'NONE',  ( 5.850189259468881353, 74.89304489562690037, 12.16667615321803808 ) ) ;
#14293 = CARTESIAN_POINT ( 'NONE',  ( 13.14645763304583070, 60.32074054053764200, 3.079995153549444975 ) ) ;
#14294 = CARTESIAN_POINT ( 'NONE',  ( 13.50000000000000000, 3.430000000000016591, 1.734723475976807094E-15 ) ) ;
#14295 = DIRECTION ( 'NONE',  ( 1.000000000000000000, 0.000000000000000000, 0.000000000000000000 ) ) ;
#14296 = CARTESIAN_POINT ( 'NONE',  ( -10.92172942406178926, 75.63000000000000966, -7.935100905948389460 ) ) ;
#14297 = CARTESIAN_POINT ( 'NONE',  ( 13.23373072280492124, 51.52419663531563998, -2.668047451998938779 ) ) ;
#14298 = CARTESIAN_POINT ( 'NONE',  ( -7.866619300871570353, 38.38328643477208146, 10.98017572201588976 ) ) ;
#14299 = CARTESIAN_POINT ( 'NONE',  ( 10.40684902343222262, 36.75901520190327432, -8.599316094126638887 ) ) ;
#14300 = CARTESIAN_POINT ( 'NONE',  ( 9.538709233711902776E-13, -44.71249999999991331, -11.37499999999999645 ) ) ;
#14301 = CARTESIAN_POINT ( 'NONE',  ( -2.617794930461571745, 74.58589864099795363, 13.24923017825046934 ) ) ;
#14302 = CARTESIAN_POINT ( 'NONE',  ( -8.912672946622391734, 77.33519948493032814, 10.14949437797439202 ) ) ;
#14303 = CARTESIAN_POINT ( 'NONE',  ( 2.494263859647128712, 62.76976130887765493, 13.26767120624862173 ) ) ;
#14304 = CARTESIAN_POINT ( 'NONE',  ( 3.083086032583709724, 41.79086483425119525, 13.14323357896869382 ) ) ;
#14305 = VERTEX_POINT ( 'NONE', #5506 ) ;
#14306 = CARTESIAN_POINT ( 'NONE',  ( -7.272992578804310604, 10.37999999999999901, 10.01041549318726709 ) ) ;
#14307 = VERTEX_POINT ( 'NONE', #12475 ) ;
#14308 = CARTESIAN_POINT ( 'NONE',  ( 9.520470885617717371, 58.73000000000000398, -6.917026985038131848 ) ) ;
#14309 = CARTESIAN_POINT ( 'NONE',  ( 1.561832610794586740E-12, -80.16249999999979536, -18.62500000000000000 ) ) ;
#14310 = CARTESIAN_POINT ( 'NONE',  ( 0.000000000000000000, 80.93000000000000682, 0.000000000000000000 ) ) ;
#14311 = CARTESIAN_POINT ( 'NONE',  ( 4.171729424061789260, -3.169999999999999041, 12.83926296998457239 ) ) ;
#14312 = EDGE_CURVE ( 'NONE', #8209, #9086, #8159, .T. ) ;
#14313 = CARTESIAN_POINT ( 'NONE',  ( 3.544998588692259478, 76.05253496923796774, -13.02654230708374605 ) ) ;
#14314 = CARTESIAN_POINT ( 'NONE',  ( -18.62500000000064659, -26.01562499999994316, 7.714727599197333419 ) ) ;
#14315 = CARTESIAN_POINT ( 'NONE',  ( -8.343458848123582072, 77.38000000000000966, 11.48378591275254124 ) ) ;
#14316 = CARTESIAN_POINT ( 'NONE',  ( 11.76794919243112325, 52.43000000000000682, 1.441158131103945434E-15 ) ) ;
#14317 = CARTESIAN_POINT ( 'NONE',  ( 8.343458848123580296, 6.980000000000003979, 11.48378591275253768 ) ) ;
#14318 = CARTESIAN_POINT ( 'NONE',  ( -10.27297386801252621, 59.26638624019382462, 8.761361963125747110 ) ) ;
#14319 = CARTESIAN_POINT ( 'NONE',  ( 13.49615201145693355, 45.41893420450175256, 0.3223442952341866174 ) ) ;
#14320 = CARTESIAN_POINT ( 'NONE',  ( 13.41772075058063152, 69.37817881389347008, 1.488226159613910360 ) ) ;
#14321 = CARTESIAN_POINT ( 'NONE',  ( -19.00000000000001776, 0.000000000000000000, 1.732050807568674466 ) ) ;
#14322 = CARTESIAN_POINT ( 'NONE',  ( 13.28728799727900700, 30.34600767625174811, 2.387053908818155712 ) ) ;
#14323 = CARTESIAN_POINT ( 'NONE',  ( -13.06985016718083514, 55.80569210471582409, -3.495749286402883627 ) ) ;
#14324 = CARTESIAN_POINT ( 'NONE',  ( -8.569946725401269561, 50.35116170713895656, 10.43101810198027657 ) ) ;
#14325 = CARTESIAN_POINT ( 'NONE',  ( 1.732050807568875195, 0.000000000000000000, -19.00000000000000000 ) ) ;
#14326 = CARTESIAN_POINT ( 'NONE',  ( 0.03720832018167305466, 43.17866651368897379, -13.49995602673501871 ) ) ;
#14327 = CARTESIAN_POINT ( 'NONE',  ( 11.95586233632780448, 39.66155393792011807, -6.269560418267513313 ) ) ;
#14328 = ORIENTED_EDGE ( 'NONE', *, *, #14586, .T. ) ;
#14329 = CARTESIAN_POINT ( 'NONE',  ( -11.17071958894546135, 61.64489015857601828, -7.580573524914104411 ) ) ;
#14330 = CARTESIAN_POINT ( 'NONE',  ( -7.272992578804307939, 6.480000000000004867, -10.01041549318726886 ) ) ;
#14331 = ORIENTED_EDGE ( 'NONE', *, *, #4492, .F. ) ;
#14332 = ORIENTED_EDGE ( 'NONE', *, *, #5116, .F. ) ;
#14333 = CARTESIAN_POINT ( 'NONE',  ( 5.883994266285501595, -19.07073825016061974, 10.19133159454443494 ) ) ;
#14334 = CARTESIAN_POINT ( 'NONE',  ( -7.714727599197335195, -5.203124999999987566, -18.62500000000064304 ) ) ;
#14335 = CARTESIAN_POINT ( 'NONE',  ( 13.20730181627872390, 48.33075532684633657, 2.806771093107235604 ) ) ;
#14336 = CARTESIAN_POINT ( 'NONE',  ( 4.749818453525196382, 58.00890527316722256, -12.63682040982544308 ) ) ;
#14337 = CARTESIAN_POINT ( 'NONE',  ( 4.128452826104092033, 79.03139843465449133, -12.85510690289249425 ) ) ;
#14338 = CARTESIAN_POINT ( 'NONE',  ( -7.576616670048093940E-16, 81.68000000000000682, 12.37355403259654985 ) ) ;
#14339 = CARTESIAN_POINT ( 'NONE',  ( 12.65542566923570256, 2.367644581053836045E-15, 2.676565841787903466 ) ) ;
#14340 = CARTESIAN_POINT ( 'NONE',  ( 13.49999999999999822, 1.279999999999994476, 4.386415899144236796 ) ) ;
#14341 = AXIS2_PLACEMENT_3D ( 'NONE', #4922, #14185, #10153 ) ;
#14342 = CARTESIAN_POINT ( 'NONE',  ( 10.12542398630638552, -99.99999999999998579, 5.924228240590371897 ) ) ;
#14343 = CARTESIAN_POINT ( 'NONE',  ( 5.883989548015876814, 30.92926152634062475, 10.19133431864935879 ) ) ;
#14344 = CARTESIAN_POINT ( 'NONE',  ( 11.37499999999960565, -41.65937499999989058, 4.711679271994918317 ) ) ;
#14345 = CARTESIAN_POINT ( 'NONE',  ( 4.171729424061789260, 43.82999999999999829, 12.83926296998457417 ) ) ;
#14346 = CARTESIAN_POINT ( 'NONE',  ( 4.453229937736239208, 34.01980578223958673, -12.74436757028742306 ) ) ;
#14347 = ORIENTED_EDGE ( 'NONE', *, *, #17408, .F. ) ;
#14348 = LINE ( 'NONE', #17012, #15419 ) ;
#14349 = ORIENTED_EDGE ( 'NONE', *, *, #7512, .T. ) ;
#14350 = CARTESIAN_POINT ( 'NONE',  ( -13.49999999999999822, 17.08000000000000540, 4.386415899144235908 ) ) ;
#14351 = CARTESIAN_POINT ( 'NONE',  ( -8.043339635996302306, -89.49374999999979252, -8.043339635997654113 ) ) ;
#14352 = MECHANICAL_DESIGN_GEOMETRIC_PRESENTATION_REPRESENTATION (  '', ( #4497 ), #4786 ) ;
#14353 = DIRECTION ( 'NONE',  ( 0.000000000000000000, 0.000000000000000000, -1.000000000000000000 ) ) ;
#14354 = CARTESIAN_POINT ( 'NONE',  ( -3.169462065277318885, 59.56607649941357607, 13.12419056553779839 ) ) ;
#14355 = CYLINDRICAL_SURFACE ( 'NONE', #15782, 4.000000000000003553 ) ;
#14356 = CARTESIAN_POINT ( 'NONE',  ( 12.50000000000000000, -14.00000000000000178, -2.204364238465235822E-15 ) ) ;
#14357 = CARTESIAN_POINT ( 'NONE',  ( -13.49999999999999822, 53.08000000000000540, 4.386415899144235908 ) ) ;
#14358 = CARTESIAN_POINT ( 'NONE',  ( -4.489412562659412131, 71.51848472666905820, 12.73166191706919825 ) ) ;
#14359 = CARTESIAN_POINT ( 'NONE',  ( 18.11581985354938595, 8.027799059190092734, -0.6932941240386443216 ) ) ;
#14360 = CARTESIAN_POINT ( 'NONE',  ( -18.62500000000000000, -91.57499999999977547, -1.562973063126292555E-12 ) ) ;
#14361 = EDGE_CURVE ( 'NONE', #8975, #3211, #10518, .T. ) ;
#14362 = CARTESIAN_POINT ( 'NONE',  ( -0.2224223267216245137, 68.67217246902345096, 13.50000000004355449 ) ) ;
#14363 = CARTESIAN_POINT ( 'NONE',  ( 1.561832610794586538E-12, -20.81249999999995026, -18.62500000000000000 ) ) ;
#14364 = CARTESIAN_POINT ( 'NONE',  ( 4.818028733689279974, 55.00634988854427831, -12.61098436172215997 ) ) ;
#14365 = CARTESIAN_POINT ( 'NONE',  ( 7.714727599200458030, -36.42187499999990763, -18.62499999999934985 ) ) ;
#14366 = CARTESIAN_POINT ( 'NONE',  ( -9.819753993301681305, 65.29014244364479680, 9.264049843067173384 ) ) ;
#14367 = CARTESIAN_POINT ( 'NONE',  ( 1.469576158976823947E-15, 102.9300000000000068, 12.00000000000000178 ) ) ;
#14368 = CARTESIAN_POINT ( 'NONE',  ( -3.926185307623118348, 35.53892993393365884, 12.91710498519315387 ) ) ;
#14369 = VERTEX_POINT ( 'NONE', #2907 ) ;
#14370 = DIRECTION ( 'NONE',  ( 0.000000000000000000, 0.000000000000000000, -1.000000000000000000 ) ) ;
#14371 = CARTESIAN_POINT ( 'NONE',  ( 7.500000000000000888, -18.00000000000000355, -2.204364238465235822E-15 ) ) ;
#14372 = CARTESIAN_POINT ( 'NONE',  ( -4.418621633216786471, 40.33892943140601517, -12.75658624249819795 ) ) ;
#14373 = CARTESIAN_POINT ( 'NONE',  ( -11.79396983171852220, 31.68639821171360893, -6.569267214410038136 ) ) ;
#14374 = PLANE ( 'NONE',  #7403 ) ;
#14375 = CARTESIAN_POINT ( 'NONE',  ( 10.46789772265251983, 60.10431960738042534, 8.525494685668089545 ) ) ;
#14376 = CARTESIAN_POINT ( 'NONE',  ( 10.92172942406179104, 1.730000000000009308, -7.935100905948385908 ) ) ;
#14377 = CARTESIAN_POINT ( 'NONE',  ( -11.06430438014261419, 53.22157550517651714, 7.735070979210682651 ) ) ;
#14378 = CARTESIAN_POINT ( 'NONE',  ( 11.76794919243112680, 55.58000000000000540, -3.823638476888993942 ) ) ;
#14379 = APPLICATION_PROTOCOL_DEFINITION ( 'draft international standard', 'automotive_design', 1998, #1448 ) ;
#14380 = CARTESIAN_POINT ( 'NONE',  ( 12.87391916192378183, 51.57647175459032240, -4.079283975827568298 ) ) ;
#14381 = CARTESIAN_POINT ( 'NONE',  ( -9.360627989232526147, 38.31329549134574108, 9.727727575345387123 ) ) ;
#14382 = AXIS2_PLACEMENT_3D ( 'NONE', #9023, #10094, #11582 ) ;
#14383 = CARTESIAN_POINT ( 'NONE',  ( 13.00679210537909469, 36.55913285882594010, -3.615981775121954289 ) ) ;
#14384 = CARTESIAN_POINT ( 'NONE',  ( 8.043339635996298753, -71.76874999999985505, 8.043339635997652337 ) ) ;
#14385 = CARTESIAN_POINT ( 'NONE',  ( -0.5999229078048249342, 74.65842898432426011, 13.48666992254756991 ) ) ;
#14386 = CARTESIAN_POINT ( 'NONE',  ( -6.382977644554325813, 77.44573456745463602, 11.89569858070153963 ) ) ;
#14387 = CARTESIAN_POINT ( 'NONE',  ( -1.768548083352462719, 80.61632827333519913, 13.38410412889483148 ) ) ;
#14388 = CARTESIAN_POINT ( 'NONE',  ( 7.500000000000000000, 108.4757119436330868, -3.584587286925195571 ) ) ;
#14389 = ORIENTED_EDGE ( 'NONE', *, *, #183, .F. ) ;
#14390 = CARTESIAN_POINT ( 'NONE',  ( 9.520470885617717371, 14.72999999999999332, -6.917026985038131848 ) ) ;
#14391 = ORIENTED_EDGE ( 'NONE', *, *, #8898, .F. ) ;
#14392 = CARTESIAN_POINT ( 'NONE',  ( 2.272985001014427393E-15, 56.17999999999999972, -12.37355403259654807 ) ) ;
#14393 = CARTESIAN_POINT ( 'NONE',  ( 9.538709233711902776E-13, -4.162499999999988987, -11.37500000000000000 ) ) ;
#14394 = PLANE ( 'NONE',  #11910 ) ;
#14395 = CARTESIAN_POINT ( 'NONE',  ( 8.605009408506106183, 75.84953091247618318, -10.40210956409493370 ) ) ;
#14396 = CARTESIAN_POINT ( 'NONE',  ( 7.714727599197339636, -80.12812499999981242, 18.62500000000063949 ) ) ;
#14397 = CARTESIAN_POINT ( 'NONE',  ( 2.319374564596460520, 65.76347162869123508, 13.30869893535136406 ) ) ;
#14398 = CARTESIAN_POINT ( 'NONE',  ( 13.50000000000000355, 72.57999999999998408, -4.386415899144233244 ) ) ;
#14399 = CARTESIAN_POINT ( 'NONE',  ( -3.636496289402153081, 47.32999999999999829, -11.19198476289190936 ) ) ;
#14400 = CARTESIAN_POINT ( 'NONE',  ( 0.000000000000000000, 80.93000000000000682, -13.50000000000000000 ) ) ;
#14401 = CARTESIAN_POINT ( 'NONE',  ( -13.49246718458698169, 58.91263165492783571, -0.5007047752432340904 ) ) ;
#14402 = EDGE_CURVE ( 'NONE', #15651, #16949, #16527, .T. ) ;
#14403 = CARTESIAN_POINT ( 'NONE',  ( 13.49839282532952289, 45.42250628188710948, 0.2187282632226159873 ) ) ;
#14404 = CARTESIAN_POINT ( 'NONE',  ( 12.93677123527108996, 69.29165259775294317, 3.862518802718706290 ) ) ;
#14405 = EDGE_CURVE ( 'NONE', #743, #4213, #15707, .T. ) ;
#14406 = CARTESIAN_POINT ( 'NONE',  ( 1.412863011855262751, 80.73080156731793977, 13.42591544637424406 ) ) ;
#14407 = CARTESIAN_POINT ( 'NONE',  ( 13.23549663901797402, 30.33587587276464248, 2.666610200634819794 ) ) ;
#14408 = CARTESIAN_POINT ( 'NONE',  ( -7.300588070086375225, 55.45236719425724203, -11.35586912590181541 ) ) ;
#14409 = CARTESIAN_POINT ( 'NONE',  ( -7.491758324924639112, 50.39954984522349690, 11.24212828544573739 ) ) ;
#14410 = CARTESIAN_POINT ( 'NONE',  ( 2.719350837857034797, 64.08222226381806763, -13.22329714325173278 ) ) ;
#14411 = CARTESIAN_POINT ( 'NONE',  ( 17.32050807568878170, 7.773118517290099838, -7.999999999999961808 ) ) ;
#14412 = CARTESIAN_POINT ( 'NONE',  ( 13.03639040501872870, 39.30446296123340488, 3.517016424516218542 ) ) ;
#14413 = ORIENTED_EDGE ( 'NONE', *, *, #14233, .F. ) ;
#14414 = CARTESIAN_POINT ( 'NONE',  ( -7.750936433791640212, 70.47186442965926290, -11.05318976959837407 ) ) ;
#14415 = CARTESIAN_POINT ( 'NONE',  ( -11.18018059938515840, 61.64547263069862026, -7.566613037985367107 ) ) ;
#14416 = CARTESIAN_POINT ( 'NONE',  ( 7.272992578804308828, 7.980000000000000426, 10.01041549318726709 ) ) ;
#14417 = ORIENTED_EDGE ( 'NONE', *, *, #2770, .T. ) ;
#14418 = CARTESIAN_POINT ( 'NONE',  ( -10.74356903153339537, 40.61907513962281513, -8.186503528442704791 ) ) ;
#14419 = VERTEX_POINT ( 'NONE', #15015 ) ;
#14420 = CARTESIAN_POINT ( 'NONE',  ( -4.171729424061791036, 26.52999999999999758, 12.83926296998457239 ) ) ;
#14421 = CARTESIAN_POINT ( 'NONE',  ( 13.16986379960055054, -2.081249999999994937, -13.16986379959834430 ) ) ;
#14422 = CARTESIAN_POINT ( 'NONE',  ( 4.718922011681848439, 47.84992210821208403, 12.64921854083997843 ) ) ;
#14423 = CARTESIAN_POINT ( 'NONE',  ( 4.756350679200790132, 58.00866332433687944, -12.63436384876514573 ) ) ;
#14424 = CARTESIAN_POINT ( 'NONE',  ( 12.58541105472228061, 78.60870476587842859, -4.931259148636751632 ) ) ;
#14425 = CARTESIAN_POINT ( 'NONE',  ( -9.520470885617717371, 75.23000000000000398, 6.917026985038133624 ) ) ;
#14426 = AXIS2_PLACEMENT_3D ( 'NONE', #16095, #8089, #15678 ) ;
#14427 = DIRECTION ( 'NONE',  ( 0.000000000000000000, 0.000000000000000000, 1.000000000000000000 ) ) ;
#14428 = ADVANCED_FACE ( 'NONE', ( #15620 ), #12563, .F. ) ;
#14429 = CARTESIAN_POINT ( 'NONE',  ( 13.49999999999999822, 41.27999999999999403, 4.386415899144236796 ) ) ;
#14430 = CARTESIAN_POINT ( 'NONE',  ( -13.50000000000000000, 33.92999999999999972, -3.306546357697853733E-15 ) ) ;
#14431 = CARTESIAN_POINT ( 'NONE',  ( -4.711679271993003404, -64.55312499999983800, -11.37500000000039613 ) ) ;
#14432 = DIRECTION ( 'NONE',  ( 0.000000000000000000, 0.000000000000000000, 1.000000000000000000 ) ) ;
#14433 = CARTESIAN_POINT ( 'NONE',  ( 5.873548170489375053, 33.96604030298396992, -12.15537189499551474 ) ) ;
#14434 = CARTESIAN_POINT ( 'NONE',  ( -12.63508156651104031, 73.75780359901375505, -4.754471429868501353 ) ) ;
#14435 = ORIENTED_EDGE ( 'NONE', *, *, #9601, .F. ) ;
#14436 = ORIENTED_EDGE ( 'NONE', *, *, #11600, .F. ) ;
#14437 = DIRECTION ( 'NONE',  ( 0.000000000000000000, -1.000000000000000000, 0.000000000000000000 ) ) ;
#14438 = ORIENTED_EDGE ( 'NONE', *, *, #11447, .T. ) ;
#14439 = CIRCLE ( 'NONE', #15556, 12.00000000000000178 ) ;
#14440 = CARTESIAN_POINT ( 'NONE',  ( 4.171729424061789260, 14.83000000000000895, 12.83926296998457239 ) ) ;
#14441 = CARTESIAN_POINT ( 'NONE',  ( 9.538709233711902776E-13, -11.41249999999998899, -11.37499999999999645 ) ) ;
#14442 = CARTESIAN_POINT ( 'NONE',  ( -0.6827152122399273715, 44.65545208943112243, 13.48272862569767661 ) ) ;
#14443 = CARTESIAN_POINT ( 'NONE',  ( -0.5990100676847840422, 59.65846358068620958, 13.48764568963964017 ) ) ;
#14444 = FACE_BOUND ( 'NONE', #10361, .T. ) ;
#14445 = DIRECTION ( 'NONE',  ( -1.000000000000000000, -0.000000000000000000, -0.000000000000000000 ) ) ;
#14446 = CARTESIAN_POINT ( 'NONE',  ( 7.752908499509820750, 66.88804938204245332, -11.05182862330812199 ) ) ;
#14447 = CARTESIAN_POINT ( 'NONE',  ( 4.171729424061791924, 55.02999999999999403, -12.83926296998457239 ) ) ;
#14448 = CARTESIAN_POINT ( 'NONE',  ( -9.316322459437627046, 71.31583036083887350, 9.780020801877546077 ) ) ;
#14449 = EDGE_CURVE ( 'NONE', #14613, #7754, #14723, .T. ) ;
#14450 = CARTESIAN_POINT ( 'NONE',  ( 7.714727599197338748, -46.82812499999989342, 18.62500000000063949 ) ) ;
#14451 = CARTESIAN_POINT ( 'NONE',  ( -1.237156021628534663, 68.63551873726167685, 13.44319788051029718 ) ) ;
#14452 = CARTESIAN_POINT ( 'NONE',  ( -18.62500000000064659, -59.31562499999985505, 7.714727599197335195 ) ) ;
#14453 = CARTESIAN_POINT ( 'NONE',  ( 9.313993393904729245, 54.81559091050048238, -9.772391642156692981 ) ) ;
#14454 = CARTESIAN_POINT ( 'NONE',  ( -3.636496289402156190, 19.53000000000001890, 11.19198476289190758 ) ) ;
#14455 = CARTESIAN_POINT ( 'NONE',  ( 18.62500000000000000, -49.94999999999988205, 1.560692158462880521E-12 ) ) ;
#14456 = CARTESIAN_POINT ( 'NONE',  ( -1.119872009197603324, 65.63978953382610371, 13.46024171269125169 ) ) ;
#14457 = CARTESIAN_POINT ( 'NONE',  ( 0.000000000000000000, 80.93000000000000682, 0.000000000000000000 ) ) ;
#14458 = CARTESIAN_POINT ( 'NONE',  ( -4.408758549868576182, 35.52142633745754097, 12.75982571945315236 ) ) ;
#14459 = VERTEX_POINT ( 'NONE', #7527 ) ;
#14460 = CARTESIAN_POINT ( 'NONE',  ( -8.891200544363830713E-16, 2.680000000000005045, 13.49999999999999822 ) ) ;
#14461 = CARTESIAN_POINT ( 'NONE',  ( -13.34948284762835158, 32.00042008344756539, 2.010355113879713329 ) ) ;
#14462 = CARTESIAN_POINT ( 'NONE',  ( 0.1489964998165439203, 73.17464263554514048, -13.49999999999999822 ) ) ;
#14463 = CARTESIAN_POINT ( 'NONE',  ( 12.41983916809079247, 60.23658299471287592, 5.309328226357375335 ) ) ;
#14464 = CARTESIAN_POINT ( 'NONE',  ( -10.92172942406179104, -8.769999999999999574, 7.935100905948385908 ) ) ;
#14465 = CARTESIAN_POINT ( 'NONE',  ( -3.713625913484355223, 53.54647381879400569, 12.97962509512433904 ) ) ;
#14466 = CARTESIAN_POINT ( 'NONE',  ( -7.272992578804310604, 54.37999999999999545, 10.01041549318726709 ) ) ;
#14467 = CARTESIAN_POINT ( 'NONE',  ( -13.50000000000000000, 75.92999999999999261, -3.306546357697853733E-15 ) ) ;
#14468 = CARTESIAN_POINT ( 'NONE',  ( 13.29424549937943389, 51.34664967739882968, 2.366107937962470320 ) ) ;
#14469 =( BOUNDED_CURVE ( )  B_SPLINE_CURVE ( 2, ( #8872, #11509, #4791, #4875, #17234, #1061, #2283, #11859, #6296, #6130, #720, #7625, #17145 ),
 .UNSPECIFIED., .F., .F. ) 
 B_SPLINE_CURVE_WITH_KNOTS ( ( 3, 2, 2, 2, 2, 2, 3 ),
 ( 0.5138888888888888395, 0.5166666666666667185, 0.5222222222222222543, 0.5277777777777777901, 0.5333333333333333259, 0.5388888888888888618, 0.5416666666666666297 ),
 .UNSPECIFIED. ) 
 CURVE ( )  GEOMETRIC_REPRESENTATION_ITEM ( )  RATIONAL_B_SPLINE_CURVE ( ( 0.9755282581475768211, 0.9755282581475762660, 1.000000000000000000, 0.9510565162951535312, 1.000000000000000000, 0.9510565162951535312, 1.000000000000000000, 0.9510565162951535312, 1.000000000000000000, 0.9510565162951535312, 1.000000000000000000, 0.9755282581475768211, 0.9755282581475768211 ) ) 
 REPRESENTATION_ITEM ( '' )  );
#14470 = CARTESIAN_POINT ( 'NONE',  ( -13.46150956673317189, 37.89473990636209066, -1.021228295727763413 ) ) ;
#14471 = CARTESIAN_POINT ( 'NONE',  ( 13.09238747814303672, 36.54713875649020594, -3.292978093212715507 ) ) ;
#14472 = CARTESIAN_POINT ( 'NONE',  ( 11.37499999999999645, -57.19999999999988916, 9.531744055041752924E-13 ) ) ;
#14473 = CARTESIAN_POINT ( 'NONE',  ( -5.218726944522628308, 74.49131902963608809, 12.45049800546231644 ) ) ;
#14474 = CARTESIAN_POINT ( 'NONE',  ( -3.791457664355128987, 77.54367317383434965, 12.95665453917505872 ) ) ;
#14475 = CARTESIAN_POINT ( 'NONE',  ( -6.837279939568707832, 80.42713201599657680, 11.64064851132507172 ) ) ;
#14476 = CARTESIAN_POINT ( 'NONE',  ( 0.000000000000000000, 80.93000000000000682, 0.000000000000000000 ) ) ;
#14477 = VERTEX_POINT ( 'NONE', #1848 ) ;
#14478 = CARTESIAN_POINT ( 'NONE',  ( 9.520470885617717371, 8.730000000000014637, -6.917026985038131848 ) ) ;
#14479 = ORIENTED_EDGE ( 'NONE', *, *, #11296, .T. ) ;
#14480 = CARTESIAN_POINT ( 'NONE',  ( 9.520470885617715595, 55.12999999999999545, 6.917026985038134512 ) ) ;
#14481 = CARTESIAN_POINT ( 'NONE',  ( -11.37500000000000178, -84.32499999999977547, -9.545674412382054647E-13 ) ) ;
#14482 = DIRECTION ( 'NONE',  ( 0.000000000000000000, 0.000000000000000000, 1.000000000000000000 ) ) ;
#14483 = CARTESIAN_POINT ( 'NONE',  ( 8.343458848123578520, -3.020000000000000462, 11.48378591275254124 ) ) ;
#14484 = CARTESIAN_POINT ( 'NONE',  ( 10.01047714262612764, 75.78048900460133552, -9.068666163624630627 ) ) ;
#14485 = CARTESIAN_POINT ( 'NONE',  ( 13.16986379959834075, -97.81874999999976694, 13.16986379960055231 ) ) ;
#14486 = CARTESIAN_POINT ( 'NONE',  ( -8.343458848123582072, 74.38000000000000966, 11.48378591275254124 ) ) ;
#14487 = CARTESIAN_POINT ( 'NONE',  ( -11.76794919243112325, 41.77999999999999403, -3.823638476888998827 ) ) ;
#14488 = CARTESIAN_POINT ( 'NONE',  ( -1.363343349470708815E-11, 9.313974596216114676, -12.00000000000000355 ) ) ;
#14489 = CARTESIAN_POINT ( 'NONE',  ( -10.94961911198126892, 59.22840902095881432, 7.897108303096641357 ) ) ;
#14490 = CARTESIAN_POINT ( 'NONE',  ( 9.130956880405868503, 45.03545779938338711, 9.943691066605332196 ) ) ;
#14491 = CARTESIAN_POINT ( 'NONE',  ( 13.42452448409018473, 69.38029835393189160, 1.426741430879768791 ) ) ;
#14492 = LINE ( 'NONE', #14321, #13993 ) ;
#14493 = CARTESIAN_POINT ( 'NONE',  ( 12.32864373793141155, 30.22870989983009338, 5.503456116662770903 ) ) ;
#14494 = CARTESIAN_POINT ( 'NONE',  ( -11.21739340954028386, 55.64777575850494884, -7.511349096803600744 ) ) ;
#14495 = CARTESIAN_POINT ( 'NONE',  ( -13.48346079216651994, 49.90693168062259133, -0.6681850952586498860 ) ) ;
#14496 = CARTESIAN_POINT ( 'NONE',  ( 4.333283499223988144, 64.02385403997206481, -12.79310945068694316 ) ) ;
#14497 = CARTESIAN_POINT ( 'NONE',  ( 8.206057751921221666, 42.86785321040926533, -10.71992093049925465 ) ) ;
#14498 = CARTESIAN_POINT ( 'NONE',  ( 11.60980040101028443, 39.17211399233057989, 6.927472449889193307 ) ) ;
#14499 = VERTEX_POINT ( 'NONE', #8599 ) ;
#14500 = CARTESIAN_POINT ( 'NONE',  ( -13.10654215744646756, 70.81327619670632600, -3.284290054994799757 ) ) ;
#14501 = CARTESIAN_POINT ( 'NONE',  ( -12.11228153988018263, 61.71073340877943991, -5.962024479802454202 ) ) ;
#14502 = ORIENTED_EDGE ( 'NONE', *, *, #4294, .T. ) ;
#14503 = AXIS2_PLACEMENT_3D ( 'NONE', #4284, #7040, #12328 ) ;
#14504 = EDGE_LOOP ( 'NONE', ( #14523, #5340, #16472, #3094 ) ) ;
#14505 = CARTESIAN_POINT ( 'NONE',  ( -13.49999999999999822, 23.08000000000000185, 4.386415899144235908 ) ) ;
#14506 = CARTESIAN_POINT ( 'NONE',  ( 7.714727599200458030, -86.37187499999978968, -18.62499999999934985 ) ) ;
#14507 = EDGE_CURVE ( 'NONE', #13385, #14181, #16876, .T. ) ;
#14508 = CARTESIAN_POINT ( 'NONE',  ( 2.439874972470002401, 61.09229787913012899, -13.28197017431443072 ) ) ;
#14509 = CARTESIAN_POINT ( 'NONE',  ( 13.36597540549724705, 57.49638167611755790, -1.897582465975046428 ) ) ;
#14510 = CARTESIAN_POINT ( 'NONE',  ( -3.636496289402153081, 65.32999999999999829, -11.19198476289190936 ) ) ;
#14511 = CARTESIAN_POINT ( 'NONE',  ( -10.92172942406178926, 36.62999999999999545, -7.935100905948389460 ) ) ;
#14512 = CARTESIAN_POINT ( 'NONE',  ( 7.272992578804308828, 75.98000000000001819, 10.01041549318726709 ) ) ;
#14513 = CARTESIAN_POINT ( 'NONE',  ( 2.970370385949144154, 7.170662809914420066, 21.14483242576215716 ) ) ;
#14514 = CARTESIAN_POINT ( 'NONE',  ( 4.878238517571312549, -99.99999999999998579, 12.54298690192642596 ) ) ;
#14515 = CARTESIAN_POINT ( 'NONE',  ( -10.92172942406178926, 75.63000000000000966, -7.935100905948389460 ) ) ;
#14516 = CARTESIAN_POINT ( 'NONE',  ( 8.043339635996302306, -90.56874999999976694, 8.043339635997654113 ) ) ;
#14517 = CARTESIAN_POINT ( 'NONE',  ( 0.000000000000000000, 80.93000000000000682, -13.50000000000000000 ) ) ;
#14518 = CARTESIAN_POINT ( 'NONE',  ( 2.040077917229468962, 34.10670120566993546, -13.35303788872347752 ) ) ;
#14519 = CARTESIAN_POINT ( 'NONE',  ( -7.490634807705651710, 73.46052964042478095, -11.23122895601197690 ) ) ;
#14520 = ORIENTED_EDGE ( 'NONE', *, *, #6829, .T. ) ;
#14521 = ORIENTED_EDGE ( 'NONE', *, *, #4596, .T. ) ;
#14522 = CARTESIAN_POINT ( 'NONE',  ( -11.76794919241189241, 80.77999999999872216, -3.823638476915469653 ) ) ;
#14523 = ORIENTED_EDGE ( 'NONE', *, *, #12638, .T. ) ;
#14524 = CARTESIAN_POINT ( 'NONE',  ( 13.50000000000000355, 12.58000000000000007, -4.386415899144233244 ) ) ;
#14525 = CARTESIAN_POINT ( 'NONE',  ( -11.37499999999999645, -65.52499999999986358, -9.545674412382054647E-13 ) ) ;
#14526 = CARTESIAN_POINT ( 'NONE',  ( -7.408466126933650031, 44.40300983023897885, 11.28560674973578060 ) ) ;
#14527 = ADVANCED_FACE ( 'NONE', ( #449 ), #5859, .F. ) ;
#14528 = CARTESIAN_POINT ( 'NONE',  ( -7.499999999999994671, -26.30006709664694853, 6.927727048493009576 ) ) ;
#14529 = CARTESIAN_POINT ( 'NONE',  ( 9.931668237600721483, 66.78434905871291960, -9.143968089697972701 ) ) ;
#14530 = CARTESIAN_POINT ( 'NONE',  ( 8.343458848123578520, 56.98000000000000398, 11.48378591275254124 ) ) ;
#14531 = CARTESIAN_POINT ( 'NONE',  ( -2.955975039020797723, 71.57371703009538066, 13.17270523474517852 ) ) ;
#14532 = VECTOR ( 'NONE', #500, 1000.000000000000000 ) ;
#14533 = CARTESIAN_POINT ( 'NONE',  ( 18.62499999999934630, -65.55937499999984652, 7.714727599200467800 ) ) ;
#14534 = CARTESIAN_POINT ( 'NONE',  ( -13.39818490939118156, 67.98779038466180680, 1.656737981020488748 ) ) ;
#14535 = CARTESIAN_POINT ( 'NONE',  ( 18.62500000000064659, 6.209375000000004974, -7.714727599197336083 ) ) ;
#14536 = CARTESIAN_POINT ( 'NONE',  ( 9.794027008236195542, 54.79149751722007267, -9.299057948655683248 ) ) ;
#14537 = CARTESIAN_POINT ( 'NONE',  ( -11.76794919243112325, 18.93000000000000327, -2.602085213965210642E-15 ) ) ;
#14538 = CARTESIAN_POINT ( 'NONE',  ( -7.714727599200467800, -44.74687499999989626, 18.62499999999934630 ) ) ;
#14539 = CARTESIAN_POINT ( 'NONE',  ( -9.781864413179627959, 65.29209033731051193, 9.304052886497448327 ) ) ;
#14540 = CARTESIAN_POINT ( 'NONE',  ( -10.92172942406179104, 43.22999999999999687, 7.935100905948387684 ) ) ;
#14541 = CARTESIAN_POINT ( 'NONE',  ( -11.24754674959912037, 35.21034174107487047, 7.466103360436171066 ) ) ;
#14542 = ORIENTED_EDGE ( 'NONE', *, *, #2873, .T. ) ;
#14543 = CARTESIAN_POINT ( 'NONE',  ( 0.000000000000000000, 9.000000000000000000, 0.000000000000000000 ) ) ;
#14544 = AXIS2_PLACEMENT_3D ( 'NONE', #3203, #15121, #7378 ) ;
#14545 = DIRECTION ( 'NONE',  ( -0.000000000000000000, 1.000000000000000000, -0.000000000000000000 ) ) ;
#14546 = EDGE_CURVE ( 'NONE', #9628, #11880, #3446, .T. ) ;
#14547 = CARTESIAN_POINT ( 'NONE',  ( 9.520470885617717371, 29.73000000000000753, -6.917026985038131848 ) ) ;
#14548 = CARTESIAN_POINT ( 'NONE',  ( -13.33720092989338646, 32.00330006321830467, 2.090426404509658553 ) ) ;
#14549 = CARTESIAN_POINT ( 'NONE',  ( 0.5655967198986255884, 73.15966327253678969, -13.48815761927076373 ) ) ;
#14550 = CARTESIAN_POINT ( 'NONE',  ( 10.65422817835172431, 60.11470094556233335, 8.290804033779142657 ) ) ;
#14551 = CARTESIAN_POINT ( 'NONE',  ( 8.343458848123583849, -7.120000000000008988, -11.48378591275253768 ) ) ;
#14552 = CARTESIAN_POINT ( 'NONE',  ( -9.915480747960748076, 53.28519106004377903, 9.161513846371878600 ) ) ;
#14553 = CARTESIAN_POINT ( 'NONE',  ( -9.520470885617715595, 53.62999999999999545, -6.917026985038136289 ) ) ;
#14554 = CARTESIAN_POINT ( 'NONE',  ( -4.171729424061787483, 75.33000000000001251, -12.83926296998457417 ) ) ;
#14555 = CARTESIAN_POINT ( 'NONE',  ( 12.48027881134552075, 51.24265653591692171, 5.147114882624049592 ) ) ;
#14556 = CIRCLE ( 'NONE', #1035, 1.999999999999998224 ) ;
#14557 = CARTESIAN_POINT ( 'NONE',  ( -11.88099997619197090, 37.69280157551202137, -6.410295481422697783 ) ) ;
#14558 = CARTESIAN_POINT ( 'NONE',  ( 10.37119814715991772, 36.76095968828544613, -8.642242444827784809 ) ) ;
#14559 = CARTESIAN_POINT ( 'NONE',  ( 4.711679271993006957, -54.07812499999989342, 11.37500000000039257 ) ) ;
#14560 = CARTESIAN_POINT ( 'NONE',  ( -2.811464633627016061E-07, 74.67999216907730897, 13.49999999999999289 ) ) ;
#14561 = CARTESIAN_POINT ( 'NONE',  ( -10.71875711079582238, 77.24165530301368676, 8.207345694687209203 ) ) ;
#14562 = CARTESIAN_POINT ( 'NONE',  ( -13.47295500694753656, 79.96043441828727794, 0.8822608226219847971 ) ) ;
#14563 = CARTESIAN_POINT ( 'NONE',  ( 3.636496289402154414, 13.83000000000000895, 11.19198476289190758 ) ) ;
#14564 = DIRECTION ( 'NONE',  ( 0.000000000000000000, 0.000000000000000000, -1.000000000000000000 ) ) ;
#14565 = ORIENTED_EDGE ( 'NONE', *, *, #16269, .F. ) ;
#14566 = CARTESIAN_POINT ( 'NONE',  ( -13.50000000000000000, 7.930000000000006821, -3.469446951953614189E-15 ) ) ;
#14567 = CARTESIAN_POINT ( 'NONE',  ( -7.272992578804307939, 12.48000000000000576, -10.01041549318726886 ) ) ;
#14568 = VERTEX_POINT ( 'NONE', #6201 ) ;
#14569 = CARTESIAN_POINT ( 'NONE',  ( -7.272992578804310604, 54.37999999999999545, 10.01041549318726886 ) ) ;
#14570 = CARTESIAN_POINT ( 'NONE',  ( 8.043339635997654113, -2.081249999999994493, -8.043339635996304082 ) ) ;
#14571 = CARTESIAN_POINT ( 'NONE',  ( 8.000000000000019540, 5.918584287042170544, -24.73863375370596174 ) ) ;
#14572 = CARTESIAN_POINT ( 'NONE',  ( 4.171729424061791924, -7.969999999999997975, -12.83926296998457239 ) ) ;
#14573 = CARTESIAN_POINT ( 'NONE',  ( 3.767968615061696003, 76.04451116420807466, -12.96361866624683579 ) ) ;
#14574 = VECTOR ( 'NONE', #11461, 1000.000000000000000 ) ;
#14575 = CARTESIAN_POINT ( 'NONE',  ( 2.138189944381259977, 67.75688142232026223, 13.49999999999999289 ) ) ;
#14576 = CARTESIAN_POINT ( 'NONE',  ( 0.6582265246141822956, 65.70366634169981523, 13.48505733660138262 ) ) ;
#14577 = CARTESIAN_POINT ( 'NONE',  ( -8.691771469529815392E-16, 74.67999999999997840, 14.19474002721660355 ) ) ;
#14578 =( BOUNDED_CURVE ( )  B_SPLINE_CURVE ( 2, ( #4507, #10171, #11309, #9914, #1831, #15606, #6106, #8847, #10087, #16947, #16862, #14203, #3514 ),
 .UNSPECIFIED., .F., .F. ) 
 B_SPLINE_CURVE_WITH_KNOTS ( ( 3, 2, 2, 2, 2, 2, 3 ),
 ( 0.5518906191050926280, 0.5547208272747723434, 0.5603812438796170747, 0.5660416604844616950, 0.5717020770893063153, 0.5773624936941509356, 0.5801927019965731347 ),
 .UNSPECIFIED. ) 
 CURVE ( )  GEOMETRIC_REPRESENTATION_ITEM ( )  RATIONAL_B_SPLINE_CURVE ( ( 0.9755282581475768211, 0.9755282592953513632, 1.000000000000000000, 0.9510565162951535312, 1.000000000000000000, 0.9510565162951535312, 1.000000000000000000, 0.9510565162951535312, 1.000000000000000000, 0.9510565162951535312, 1.000000000000000000, 0.9755282581475777093, 0.9755282581475767101 ) ) 
 REPRESENTATION_ITEM ( '' )  );
#14579 = CARTESIAN_POINT ( 'NONE',  ( 9.520470885617717371, 37.72999999999999687, -6.917026985038131848 ) ) ;
#14580 = CARTESIAN_POINT ( 'NONE',  ( 17.32050807568873552, 0.000000000000000000, 8.000000000000085265 ) ) ;
#14581 = CARTESIAN_POINT ( 'NONE',  ( -12.68991400004249392, 58.76347348998390885, -4.606612073962529585 ) ) ;
#14582 = CARTESIAN_POINT ( 'NONE',  ( 10.41641641675877139, 45.10151672092631969, 8.587682018090683655 ) ) ;
#14583 = CARTESIAN_POINT ( 'NONE',  ( 12.80716480624030496, 69.27630802522288889, 4.269263623378532380 ) ) ;
#14584 = CARTESIAN_POINT ( 'NONE',  ( -8.343458848123578520, 66.48000000000000398, -11.48378591275254124 ) ) ;
#14585 = DIRECTION ( 'NONE',  ( -1.000000000000000000, -0.000000000000000000, -0.000000000000000000 ) ) ;
#14586 = EDGE_CURVE ( 'NONE', #10383, #17140, #15535, .T. ) ;
#14587 = CARTESIAN_POINT ( 'NONE',  ( -0.6538802958928384701, 55.20351089476487516, -13.48419838928958292 ) ) ;
#14588 = CARTESIAN_POINT ( 'NONE',  ( -10.60346985883564841, 50.24833156966194991, 8.358339015696030216 ) ) ;
#14589 = CARTESIAN_POINT ( 'NONE',  ( 9.817055075673792430, 63.79028200361416623, -9.266916700068716040 ) ) ;
#14590 = CARTESIAN_POINT ( 'NONE',  ( 12.99972812561954250, 42.56007091286085142, -3.641089568116410824 ) ) ;
#14591 = CARTESIAN_POINT ( 'NONE',  ( 9.430394439940833706, 39.05013839999956815, 9.660559727168038791 ) ) ;
#14592 = EDGE_LOOP ( 'NONE', ( #7686, #6314, #4768, #11635 ) ) ;
#14593 = CARTESIAN_POINT ( 'NONE',  ( -9.817573801958880964, 70.56979445902175030, -9.266430505722183852 ) ) ;
#14594 = CARTESIAN_POINT ( 'NONE',  ( -11.16425593428273189, 61.64449276969597946, -7.590094044152214892 ) ) ;
#14595 = CARTESIAN_POINT ( 'NONE',  ( 9.520470885617717371, 5.730000000000012861, -6.917026985038131848 ) ) ;
#14596 = ORIENTED_EDGE ( 'NONE', *, *, #14132, .F. ) ;
#14597 = EDGE_LOOP ( 'NONE', ( #12397, #16970, #4080, #8972 ) ) ;
#14598 = CARTESIAN_POINT ( 'NONE',  ( -8.343458848123576743, 22.48000000000000753, -11.48378591275254301 ) ) ;
#14599 = CARTESIAN_POINT ( 'NONE',  ( -18.62499999999934985, -40.58437499999990905, -7.714727599200458918 ) ) ;
#14600 = CARTESIAN_POINT ( 'NONE',  ( 3.179672653360267720, 61.06567017344302428, -13.12035135455492885 ) ) ;
#14601 = CARTESIAN_POINT ( 'NONE',  ( 10.66243950754257419, 72.11517382313176938, 8.280248928875550973 ) ) ;
#14602 = CARTESIAN_POINT ( 'NONE',  ( 13.48635267069885479, 57.45126414530135861, -0.6183634171442978777 ) ) ;
#14603 = CARTESIAN_POINT ( 'NONE',  ( 7.272992578804308828, 66.98000000000000398, 10.01041549318726709 ) ) ;
#14604 = CARTESIAN_POINT ( 'NONE',  ( -7.272992578804310604, 75.37999999999999545, 10.01041549318726709 ) ) ;
#14605 = DIRECTION ( 'NONE',  ( -0.000000000000000000, -1.000000000000000000, -0.000000000000000000 ) ) ;
#14606 = CARTESIAN_POINT ( 'NONE',  ( 8.343458848123583849, 38.87999999999998835, -11.48378591275253768 ) ) ;
#14607 = CARTESIAN_POINT ( 'NONE',  ( -10.92172942406178926, 33.63000000000000256, -7.935100905948389460 ) ) ;
#14608 = CARTESIAN_POINT ( 'NONE',  ( -11.37500000000039790, -68.71562499999981810, 4.711679271993001628 ) ) ;
#14609 = CARTESIAN_POINT ( 'NONE',  ( 15.00000000000000000, -99.89999999999999147, 0.000000000000000000 ) ) ;
#14610 = CARTESIAN_POINT ( 'NONE',  ( 5.829534447797559693, 33.96776797207451892, -12.17648583204983659 ) ) ;
#14611 = CARTESIAN_POINT ( 'NONE',  ( -10.35327952210849922, 73.59810291917281688, -8.665258164064150392 ) ) ;
#14612 = VERTEX_POINT ( 'NONE', #4607 ) ;
#14613 = VERTEX_POINT ( 'NONE', #9927 ) ;
#14614 = CARTESIAN_POINT ( 'NONE',  ( -9.520470885617717371, 75.23000000000000398, 6.917026985038133624 ) ) ;
#14615 = ORIENTED_EDGE ( 'NONE', *, *, #14507, .T. ) ;
#14616 = CARTESIAN_POINT ( 'NONE',  ( -4.711679271994915652, -51.99687499999990337, 11.37499999999960210 ) ) ;
#14617 = CARTESIAN_POINT ( 'NONE',  ( -7.499999999999993783, -25.08364130939904157, -8.254396200996691135 ) ) ;
#14618 = CARTESIAN_POINT ( 'NONE',  ( 13.40118537505952467, 66.48685356940795543, -1.630447449414718974 ) ) ;
#14619 = VECTOR ( 'NONE', #4671, 1000.000000000000000 ) ;
#14620 = CARTESIAN_POINT ( 'NONE',  ( 4.171729424061789260, 41.82999999999999829, 12.83926296998457417 ) ) ;
#14621 = CARTESIAN_POINT ( 'NONE',  ( -11.57172165442571199, 71.18898023797920871, 6.959135939452125719 ) ) ;
#14622 = CARTESIAN_POINT ( 'NONE',  ( -13.16986379959834252, -72.84374999999981526, -13.16986379960055054 ) ) ;
#14623 = CARTESIAN_POINT ( 'NONE',  ( -12.75392120890703751, 68.08976633361912434, 4.429612562818754817 ) ) ;
#14624 = CARTESIAN_POINT ( 'NONE',  ( -7.714727599200466912, -20.84687499999993321, 18.62499999999935341 ) ) ;
#14625 = EDGE_CURVE ( 'NONE', #39, #717, #3755, .T. ) ;
#14626 = CARTESIAN_POINT ( 'NONE',  ( 10.49117977328117668, 54.75438394012941501, -8.496252905792848864 ) ) ;
#14627 = CARTESIAN_POINT ( 'NONE',  ( 3.636496289402154414, 16.83000000000001251, 11.19198476289190758 ) ) ;
#14628 = CARTESIAN_POINT ( 'NONE',  ( 1.561832610794586538E-12, -87.41249999999979536, -18.62500000000000000 ) ) ;
#14629 = CARTESIAN_POINT ( 'NONE',  ( -13.42050307411934895, 64.98104791279109804, 1.467013915166769822 ) ) ;
#14630 = CARTESIAN_POINT ( 'NONE',  ( -4.449551195726444419, 35.51993990970242265, 12.74565100145505703 ) ) ;
#14631 = CARTESIAN_POINT ( 'NONE',  ( -8.343458848123576743, 20.47999999999999687, -11.48378591275254301 ) ) ;
#14632 = ORIENTED_EDGE ( 'NONE', *, *, #12334, .T. ) ;
#14633 = DIRECTION ( 'NONE',  ( 0.000000000000000000, -1.000000000000000000, 0.000000000000000000 ) ) ;
#14634 = CARTESIAN_POINT ( 'NONE',  ( -3.636496289402152637, 27.32999999999999474, -11.19198476289190936 ) ) ;
#14635 = CARTESIAN_POINT ( 'NONE',  ( -5.494845225242961817, 31.37922778511446964, -12.33112964525436439 ) ) ;
#14636 = DIRECTION ( 'NONE',  ( 6.313931023057710304E-15, 0.000000000000000000, -1.000000000000000000 ) ) ;
#14637 = CARTESIAN_POINT ( 'NONE',  ( 11.69961049517324625, 60.17965554828174390, 6.735864183870432065 ) ) ;
#14638 = B_SPLINE_CURVE_WITH_KNOTS ( 'NONE', 3,
 ( #3326, #8741, #1983, #14099, #17019, #3415, #7409, #6089, #12791, #677, #11469, #16845, #8828, #7671, #4923, #14186, #8914, #11555 ),
 .UNSPECIFIED., .F., .F.,
 ( 4, 2, 2, 2, 2, 2, 2, 2, 4 ),
 ( 2.030049010680398490E-07, 0.0005272941439305970247, 0.001054385282960126164, 0.001581476421989655087, 0.002108567561019184227, 0.002635658700048713367, 0.003162749839078242073, 0.003689840978107771213, 0.004216932117137300352 ),
 .UNSPECIFIED. ) ;
#14639 = CARTESIAN_POINT ( 'NONE',  ( -7.243158421774579914, 53.41008471037572747, 11.39280974719889272 ) ) ;
#14640 = AXIS2_PLACEMENT_3D ( 'NONE', #15518, #11400, #8846 ) ;
#14641 = CARTESIAN_POINT ( 'NONE',  ( 11.76794919243112325, 52.28000000000000114, 3.823638476888996607 ) ) ;
#14642 = CARTESIAN_POINT ( 'NONE',  ( -4.171729424061787483, 69.32999999999999829, -12.83926296998457417 ) ) ;
#14643 = CARTESIAN_POINT ( 'NONE',  ( 3.382362776236492508, 50.80156238092428111, 13.06946539059775425 ) ) ;
#14644 = CARTESIAN_POINT ( 'NONE',  ( -13.26641961833640160, 37.84148543181640179, -2.512961166757757159 ) ) ;
#14645 = CARTESIAN_POINT ( 'NONE',  ( 10.88107893182741925, 36.12754488146830312, 7.991670572652272320 ) ) ;
#14646 = CARTESIAN_POINT ( 'NONE',  ( -8.043339635997652337, -100.9062499999997868, 8.043339635996300530 ) ) ;
#14647 = CARTESIAN_POINT ( 'NONE',  ( -5.224982848479887920, 74.49108573728641147, 12.44787394451754281 ) ) ;
#14648 = CARTESIAN_POINT ( 'NONE',  ( -12.50942665065559289, 76.74541654896083287, -5.075876066077060322 ) ) ;
#14649 = CARTESIAN_POINT ( 'NONE',  ( -8.910189170011362236, 80.33521782052793014, 10.14428475681184416 ) ) ;
#14650 = CARTESIAN_POINT ( 'NONE',  ( 7.272992578804308828, 10.98000000000000576, 10.01041549318726709 ) ) ;
#14651 = CARTESIAN_POINT ( 'NONE',  ( 7.500000000000000888, 103.4443346693207957, 9.346209313438659905 ) ) ;
#14652 = CARTESIAN_POINT ( 'NONE',  ( 7.500000000000000888, 98.93000000000002103, -8.999999999999996447 ) ) ;
#14653 = CARTESIAN_POINT ( 'NONE',  ( -7.272992578804307939, 6.480000000000004867, -10.01041549318726886 ) ) ;
#14654 = CARTESIAN_POINT ( 'NONE',  ( 11.76794919243112325, 52.43000000000000682, 1.441158131103945434E-15 ) ) ;
#14655 = CARTESIAN_POINT ( 'NONE',  ( 9.538709233711902776E-13, -63.51249999999981810, -11.37500000000000178 ) ) ;
#14656 = CARTESIAN_POINT ( 'NONE',  ( -7.714727599200467800, -11.44687499999997371, 18.62499999999934630 ) ) ;
#14657 = CARTESIAN_POINT ( 'NONE',  ( 10.92172942406179104, -11.26999999999999602, -7.935100905948385908 ) ) ;
#14658 = CARTESIAN_POINT ( 'NONE',  ( 13.50000000000000000, 35.42999999999999972, 1.653273178848926867E-15 ) ) ;
#14659 = CARTESIAN_POINT ( 'NONE',  ( 8.034607623683875488, 75.87556492978765732, -10.85026718143496183 ) ) ;
#14660 = DIRECTION ( 'NONE',  ( 0.000000000000000000, 0.000000000000000000, 1.000000000000000000 ) ) ;
#14661 = CARTESIAN_POINT ( 'NONE',  ( -3.636496289402155746, 36.53000000000000114, 11.19198476289190936 ) ) ;
#14662 = DIRECTION ( 'NONE',  ( -1.000000000000000000, -0.000000000000000000, -0.000000000000000000 ) ) ;
#14663 = CARTESIAN_POINT ( 'NONE',  ( -11.13715108135233400, 58.64282742455466746, -7.629921315917804314 ) ) ;
#14664 = CARTESIAN_POINT ( 'NONE',  ( -5.485275766071775660E-07, 44.67998473833578998, 13.49999999999997691 ) ) ;
#14665 = CARTESIAN_POINT ( 'NONE',  ( 12.99932277953478987, 69.56086486162749338, -3.664194174932866144 ) ) ;
#14666 = ADVANCED_FACE ( 'NONE', ( #3268 ), #14044, .T. ) ;
#14667 = CARTESIAN_POINT ( 'NONE',  ( 0.000000000000000000, -28.00000000000000000, 12.00000000000000178 ) ) ;
#14668 = CARTESIAN_POINT ( 'NONE',  ( 12.50000000000000000, 98.93000000000002103, -8.999999999999996447 ) ) ;
#14669 = CARTESIAN_POINT ( 'NONE',  ( -1.222984669013519099, 55.22395752754145803, -13.44686810295633173 ) ) ;
#14670 = CARTESIAN_POINT ( 'NONE',  ( -8.726673703696462780, 50.34384715345172623, 10.30054475047543505 ) ) ;
#14671 = CARTESIAN_POINT ( 'NONE',  ( 13.34146757976997932, 63.50243722178738892, -2.066615361868207934 ) ) ;
#14672 = CARTESIAN_POINT ( 'NONE',  ( 13.08065693840681121, 42.54885315171381421, -3.339269834337736054 ) ) ;
#14673 = CARTESIAN_POINT ( 'NONE',  ( 9.236967615830064204, 39.04062162967218086, 9.845233498274197359 ) ) ;
#14674 = ORIENTED_EDGE ( 'NONE', *, *, #3581, .T. ) ;
#14675 = CARTESIAN_POINT ( 'NONE',  ( -9.784440633357435857, 70.56809849894560216, -9.301509274256069659 ) ) ;
#14676 = DIRECTION ( 'NONE',  ( 0.000000000000000000, 0.000000000000000000, -1.000000000000000000 ) ) ;
#14677 = CARTESIAN_POINT ( 'NONE',  ( -11.76794919243112325, 7.080000000000000959, 3.823638476888994386 ) ) ;
#14678 = VERTEX_POINT ( 'NONE', #6033 ) ;
#14679 = EDGE_LOOP ( 'NONE', ( #15717, #11742, #10724, #7268 ) ) ;
#14680 = CARTESIAN_POINT ( 'NONE',  ( 4.171729424061791924, 19.03000000000001890, -12.83926296998457239 ) ) ;
#14681 = CARTESIAN_POINT ( 'NONE',  ( -7.714727599197335195, -55.15312499999986784, -18.62500000000064304 ) ) ;
#14682 = CARTESIAN_POINT ( 'NONE',  ( -10.92172942406179104, 15.22999999999999332, 7.935100905948385908 ) ) ;
#14683 = CARTESIAN_POINT ( 'NONE',  ( 10.17113817942703946, 72.08819647464973457, 8.881040390352081815 ) ) ;
#14684 = CARTESIAN_POINT ( 'NONE',  ( 12.15229061391567633, 57.21392339986990550, 5.883136067267471070 ) ) ;
#14685 = B_SPLINE_CURVE_WITH_KNOTS ( 'NONE', 3,
 ( #4936, #7509, #7428, #2344, #13062, #10336 ),
 .UNSPECIFIED., .F., .F.,
 ( 4, 2, 4 ),
 ( 0.003156405538531764036, 0.003686668827834532411, 0.004216932117137300352 ),
 .UNSPECIFIED. ) ;
#14686 = CARTESIAN_POINT ( 'NONE',  ( -9.520470885617717371, 69.23000000000000398, 6.917026985038133624 ) ) ;
#14687 = CARTESIAN_POINT ( 'NONE',  ( 9.520470885617715595, 73.12999999999999545, 6.917026985038134512 ) ) ;
#14688 = CARTESIAN_POINT ( 'NONE',  ( -6.660722695897963952, 47.43442504079767019, 11.74429954586069158 ) ) ;
#14689 = CARTESIAN_POINT ( 'NONE',  ( -13.50000000000000000, 45.92999999999999972, -3.306546357697853733E-15 ) ) ;
#14690 = CARTESIAN_POINT ( 'NONE',  ( 1.732050807568875195, 0.000000000000000000, -19.00000000000000000 ) ) ;
#14691 = CARTESIAN_POINT ( 'NONE',  ( 4.063219964874296153, 10.00000000000000000, -12.84931952050321868 ) ) ;
#14692 = CARTESIAN_POINT ( 'NONE',  ( -4.711679271994916540, -87.44687499999976410, 11.37499999999960565 ) ) ;
#14693 = DIRECTION ( 'NONE',  ( 0.000000000000000000, 0.000000000000000000, 1.000000000000000000 ) ) ;
#14694 = CARTESIAN_POINT ( 'NONE',  ( 13.50053299712392985, 33.42724656409518502, 0.07573446942323454334 ) ) ;
#14695 = CARTESIAN_POINT ( 'NONE',  ( -2.111840279952809762, 73.25593118054010233, -13.33386240694283664 ) ) ;
#14696 = EDGE_LOOP ( 'NONE', ( #821, #17446, #9889, #4727 ) ) ;
#14697 = VERTEX_POINT ( 'NONE', #3528 ) ;
#14698 = CARTESIAN_POINT ( 'NONE',  ( -9.520470885617715595, 80.63000000000000966, -6.917026985038136289 ) ) ;
#14699 = ORIENTED_EDGE ( 'NONE', *, *, #12599, .T. ) ;
#14700 = CARTESIAN_POINT ( 'NONE',  ( 11.37499999999960210, -89.45937499999983800, 4.711679271994916540 ) ) ;
#14701 = CARTESIAN_POINT ( 'NONE',  ( 9.154805866618415777, 8.062143943920768052, 15.49921147158547186 ) ) ;
#14702 = EDGE_CURVE ( 'NONE', #7842, #16820, #8001, .T. ) ;
#14703 = CARTESIAN_POINT ( 'NONE',  ( 13.50000000000000000, 39.42999999999999972, 1.653273178848926867E-15 ) ) ;
#14704 = CARTESIAN_POINT ( 'NONE',  ( -11.94380634845912859, 71.16263373931494129, 6.294515196234966581 ) ) ;
#14705 = B_SPLINE_CURVE_WITH_KNOTS ( 'NONE', 3,
 ( #6887, #9541, #5379, #13319 ),
 .UNSPECIFIED., .F., .F.,
 ( 4, 4 ),
 ( 2.383248697869602982E-07, 0.007646667935218605036 ),
 .UNSPECIFIED. ) ;
#14706 = CARTESIAN_POINT ( 'NONE',  ( 18.62499999999935341, -58.30937499999983231, 7.714727599200469577 ) ) ;
#14707 = CARTESIAN_POINT ( 'NONE',  ( -11.74368838437089124, 68.17729472189647311, 6.658789978823069333 ) ) ;
#14708 = CARTESIAN_POINT ( 'NONE',  ( -13.16986379959834252, -89.49374999999979252, -13.16986379960055054 ) ) ;
#14709 = AXIS2_PLACEMENT_3D ( 'NONE', #9368, #1041, #17125 ) ;
#14710 = CARTESIAN_POINT ( 'NONE',  ( 11.60265521985991022, 54.68715047374503513, -6.901813903172819842 ) ) ;
#14711 = CARTESIAN_POINT ( 'NONE',  ( -7.272992578804307939, 21.48000000000001108, -10.01041549318726886 ) ) ;
#14712 = CARTESIAN_POINT ( 'NONE',  ( 18.62500000000000000, -83.24999999999980105, 1.560692158462880521E-12 ) ) ;
#14713 = CARTESIAN_POINT ( 'NONE',  ( -13.13342003293556637, 64.81895280616910782, -3.128236002867767596 ) ) ;
#14714 = CARTESIAN_POINT ( 'NONE',  ( -9.846957267435957561, 35.28912329287517480, 9.246335277936564623 ) ) ;
#14715 = ORIENTED_EDGE ( 'NONE', *, *, #3486, .F. ) ;
#14716 = CARTESIAN_POINT ( 'NONE',  ( -4.130660464442061475, 2.022510465845311355E-14, -11.65984581473472836 ) ) ;
#14717 = CARTESIAN_POINT ( 'NONE',  ( -5.478259550403512534, 31.37858928543126780, -12.33850698730843654 ) ) ;
#14718 = CARTESIAN_POINT ( 'NONE',  ( 13.14483242576204880, 7.170662809914418290, 16.82677684650038330 ) ) ;
#14719 = CARTESIAN_POINT ( 'NONE',  ( 4.330177564208073981, 59.83558484829251967, 12.78997803238905995 ) ) ;
#14720 = ADVANCED_FACE ( 'NONE', ( #11416 ), #16788, .T. ) ;
#14721 = CARTESIAN_POINT ( 'NONE',  ( 10.92172942406178926, -7.869999999999994778, 7.935100905948385908 ) ) ;
#14722 = CARTESIAN_POINT ( 'NONE',  ( -7.142235745276270364, 53.41435411266112254, 11.45593642778781351 ) ) ;
#14723 = CIRCLE ( 'NONE', #7433, 13.50000000000000000 ) ;
#14724 = CARTESIAN_POINT ( 'NONE',  ( -7.576616670048093940E-16, 48.67999999999999261, 12.37355403259654985 ) ) ;
#14725 = CARTESIAN_POINT ( 'NONE',  ( 8.343458848123583849, 68.88000000000000966, -11.48378591275253768 ) ) ;
#14726 = CARTESIAN_POINT ( 'NONE',  ( 10.77064554674818275, 51.12129249041564805, 8.139387900364980055 ) ) ;
#14727 = CARTESIAN_POINT ( 'NONE',  ( -7.795330123696450286, 37.47372399862477721, -11.02641059027264347 ) ) ;
#14728 = CARTESIAN_POINT ( 'NONE',  ( 13.32600202517275179, 36.35416429240112990, 2.160700448193091816 ) ) ;
#14729 = CARTESIAN_POINT ( 'NONE',  ( 1.561832610794586740E-12, -11.41249999999999254, -18.62500000000000000 ) ) ;
#14730 = CARTESIAN_POINT ( 'NONE',  ( -8.576537068151989018, 74.35087396422935058, 10.42646147084938768 ) ) ;
#14731 = CARTESIAN_POINT ( 'NONE',  ( -13.45696768390258313, 76.96804991183022082, 1.099532284017214367 ) ) ;
#14732 = AXIS2_PLACEMENT_3D ( 'NONE', #11488, #5929, #3347 ) ;
#14733 = CARTESIAN_POINT ( 'NONE',  ( -12.38291575527968469, 80.12633443854863913, 5.378268875544708116 ) ) ;
#14734 = CARTESIAN_POINT ( 'NONE',  ( -3.636496289402152637, 12.33000000000000718, -11.19198476289190936 ) ) ;
#14735 = CARTESIAN_POINT ( 'NONE',  ( 7.499999999999999112, 108.1058439696177373, -5.080312676971233010 ) ) ;
#14736 = DIRECTION ( 'NONE',  ( 0.000000000000000000, -1.000000000000000000, 0.000000000000000000 ) ) ;
#14737 = CARTESIAN_POINT ( 'NONE',  ( -9.520470885617715595, 0.6299999999999916778, -6.917026985038136289 ) ) ;
#14738 = CARTESIAN_POINT ( 'NONE',  ( -7.272992578804310604, 45.38000000000000256, 10.01041549318726886 ) ) ;
#14739 = CARTESIAN_POINT ( 'NONE',  ( 11.37500000000000000, -33.29999999999991900, 9.531744055041752924E-13 ) ) ;
#14740 = CARTESIAN_POINT ( 'NONE',  ( 18.62500000000064304, -17.69062499999995453, -7.714727599197335195 ) ) ;
#14741 = CARTESIAN_POINT ( 'NONE',  ( -4.171729424061787483, -10.66999999999999815, -12.83926296998457417 ) ) ;
#14742 = CARTESIAN_POINT ( 'NONE',  ( -10.19991245802031798, 40.58986062522050275, -8.843942352183722377 ) ) ;
#14743 = LINE ( 'NONE', #17487, #654 ) ;
#14744 = CARTESIAN_POINT ( 'NONE',  ( 12.92208239490048882, 75.57016071826951986, -3.911420954987763210 ) ) ;
#14745 = ADVANCED_FACE ( 'NONE', ( #7444 ), #12823, .F. ) ;
#14746 = FACE_OUTER_BOUND ( 'NONE', #483, .T. ) ;
#14747 = CARTESIAN_POINT ( 'NONE',  ( 9.520470885617717371, 40.72999999999999687, -6.917026985038131848 ) ) ;
#14748 = CARTESIAN_POINT ( 'NONE',  ( -3.295356814209294605, 41.56178627527702929, 13.09792834740329681 ) ) ;
#14749 = CARTESIAN_POINT ( 'NONE',  ( -12.80432099898033727, 58.77598328227021085, -4.277830564778782652 ) ) ;
#14750 = CARTESIAN_POINT ( 'NONE',  ( 4.545821450575014744, 44.84357583826527360, 12.71174574629005960 ) ) ;
#14751 = CARTESIAN_POINT ( 'NONE',  ( -24.73863375370603634, 5.918584287042171432, 7.999999999999761080 ) ) ;
#14752 = CARTESIAN_POINT ( 'NONE',  ( 10.00000000000135891, 7.983052681821872554, -15.32050807568352191 ) ) ;
#14753 = CARTESIAN_POINT ( 'NONE',  ( -10.45946617061218475, 55.60358966935245917, -8.539753337778272169 ) ) ;
#14754 = CARTESIAN_POINT ( 'NONE',  ( -10.13059983448895807, 49.58610714942754782, -8.923059655268989587 ) ) ;
#14755 = CARTESIAN_POINT ( 'NONE',  ( 11.50193147421984641, 63.69388881605808450, -7.067926430401910487 ) ) ;
#14756 = CARTESIAN_POINT ( 'NONE',  ( 11.16643148321324830, 42.71536710878835663, -7.586896124391933505 ) ) ;
#14757 = CARTESIAN_POINT ( 'NONE',  ( 8.740268137309426422, 39.01678215043063602, 10.29112316391600856 ) ) ;
#14758 = ORIENTED_EDGE ( 'NONE', *, *, #11562, .F. ) ;
#14759 = CARTESIAN_POINT ( 'NONE',  ( -9.938187692555990438, 70.57591519484154219, -9.136943841256590204 ) ) ;
#14760 = CARTESIAN_POINT ( 'NONE',  ( 2.445080149700053643E-15, 48.17999999999999972, -13.50000000000000000 ) ) ;
#14761 = ORIENTED_EDGE ( 'NONE', *, *, #4043, .F. ) ;
#14762 = ORIENTED_EDGE ( 'NONE', *, *, #17050, .F. ) ;
#14763 = CARTESIAN_POINT ( 'NONE',  ( -8.343458848123576743, 19.48000000000000043, -11.48378591275254301 ) ) ;
#14764 = CARTESIAN_POINT ( 'NONE',  ( -7.714727599200467800, -61.39687499999984510, 18.62499999999934630 ) ) ;
#14765 = CARTESIAN_POINT ( 'NONE',  ( 3.290941839471703378, 47.79834429727236511, 13.09273932709712263 ) ) ;
#14766 = CARTESIAN_POINT ( 'NONE',  ( 10.92172942406178926, 13.13000000000000256, 7.935100905948385908 ) ) ;
#14767 = EDGE_CURVE ( 'NONE', #8561, #1210, #16391, .T. ) ;
#14768 = CARTESIAN_POINT ( 'NONE',  ( 9.091042220740154889, 72.03320402041192949, 9.992426890892799562 ) ) ;
#14769 = CARTESIAN_POINT ( 'NONE',  ( 11.89283365199842812, 57.66647961388354560, -6.391320871232198719 ) ) ;
#14770 = CARTESIAN_POINT ( 'NONE',  ( 11.76794919243112325, 64.43000000000000682, 1.441158131103945434E-15 ) ) ;
#14771 = CARTESIAN_POINT ( 'NONE',  ( -8.691771469529815392E-16, 34.67999999999999972, 14.19474002721660355 ) ) ;
#14772 = CARTESIAN_POINT ( 'NONE',  ( 3.636496289402154414, 78.82999999999999829, 11.19198476289190936 ) ) ;
#14773 = CARTESIAN_POINT ( 'NONE',  ( -7.710663883636067695, 47.38997137728517117, 11.08260043313612542 ) ) ;
#14774 = LINE ( 'NONE', #2664, #7315 ) ;
#14775 = CARTESIAN_POINT ( 'NONE',  ( 2.138189944381242213, 39.10311857767973009, -13.49999999999999822 ) ) ;
#14776 = CARTESIAN_POINT ( 'NONE',  ( 2.000520122481862502E-14, 76.67999999999999261, 13.50000000000000000 ) ) ;
#14777 = CARTESIAN_POINT ( 'NONE',  ( -4.711679271994916540, -70.79687499999981526, 11.37499999999960565 ) ) ;
#14778 = CARTESIAN_POINT ( 'NONE',  ( -13.49999999999999822, 52.07999999999999119, 4.386415899144235020 ) ) ;
#14779 = CARTESIAN_POINT ( 'NONE',  ( 13.46464982345765371, 33.46446917462228754, -0.9962107245471286676 ) ) ;
#14780 = CARTESIAN_POINT ( 'NONE',  ( -4.994567026383744057, 73.36021605965370895, -12.54210557001517756 ) ) ;
#14781 = ORIENTED_EDGE ( 'NONE', *, *, #4716, .T. ) ;
#14782 = ORIENTED_EDGE ( 'NONE', *, *, #10114, .F. ) ;
#14783 =( BOUNDED_CURVE ( )  B_SPLINE_CURVE ( 2, ( #11045, #9729, #15582, #11631, #5665, #1569, #6988, #3490, #4319, #16594, #15075, #12363, #15167 ),
 .UNSPECIFIED., .F., .F. ) 
 B_SPLINE_CURVE_WITH_KNOTS ( ( 3, 2, 2, 2, 2, 2, 3 ),
 ( 0.5138888888888888395, 0.5166666666666667185, 0.5222222222222222543, 0.5277777777777777901, 0.5333333333333333259, 0.5388888888888888618, 0.5416666666666666297 ),
 .UNSPECIFIED. ) 
 CURVE ( )  GEOMETRIC_REPRESENTATION_ITEM ( )  RATIONAL_B_SPLINE_CURVE ( ( 0.9755282581475768211, 0.9755282581475762660, 1.000000000000000000, 0.9510565162951535312, 1.000000000000000000, 0.9510565162951535312, 1.000000000000000000, 0.9510565162951535312, 1.000000000000000000, 0.9510565162951535312, 1.000000000000000000, 0.9755282581475768211, 0.9755282581475768211 ) ) 
 REPRESENTATION_ITEM ( '' )  );
#14784 = ORIENTED_EDGE ( 'NONE', *, *, #9164, .T. ) ;
#14785 = CARTESIAN_POINT ( 'NONE',  ( -13.32596712241149461, 41.00582476662071940, 2.160751794978737372 ) ) ;
#14786 = CARTESIAN_POINT ( 'NONE',  ( -8.043339635996300530, -63.44374999999985931, -8.043339635997652337 ) ) ;
#14787 = CARTESIAN_POINT ( 'NONE',  ( 1.653273178848926472E-15, 30.93000000000001393, 13.50000000000000000 ) ) ;
#14788 = CARTESIAN_POINT ( 'NONE',  ( -7.499999999999993783, -27.54571194363307995, -3.584587286925202232 ) ) ;
#14789 = CARTESIAN_POINT ( 'NONE',  ( 10.92172942406178926, 39.12999999999999545, 7.935100905948387684 ) ) ;
#14790 = CARTESIAN_POINT ( 'NONE',  ( -12.86018314841378363, 71.07761088014338213, 4.108712978716644315 ) ) ;
#14791 = CARTESIAN_POINT ( 'NONE',  ( 18.62500000000064659, -27.09062499999992113, -7.714727599197336083 ) ) ;
#14792 = CARTESIAN_POINT ( 'NONE',  ( -12.47230674160408981, 67.74175760280583347, -5.171836198928197348 ) ) ;
#14793 = CARTESIAN_POINT ( 'NONE',  ( 18.62500000000000000, 7.250000000000001776, 1.560692158462880521E-12 ) ) ;
#14794 = CARTESIAN_POINT ( 'NONE',  ( 11.86106144339729696, 54.66890001434251900, -6.452874835814393251 ) ) ;
#14795 = CARTESIAN_POINT ( 'NONE',  ( -11.76794919243112325, 15.92999999999999972, -2.602085213965210642E-15 ) ) ;
#14796 = CYLINDRICAL_SURFACE ( 'NONE', #8738, 13.50000000000000000 ) ;
#14797 = EDGE_CURVE ( 'NONE', #6661, #9217, #12016, .T. ) ;
#14798 = CARTESIAN_POINT ( 'NONE',  ( -13.31844401820848844, 65.00776987222435821, 2.214491255749064358 ) ) ;
#14799 = CARTESIAN_POINT ( 'NONE',  ( -13.02318491043671500, 34.80308345404688453, -3.556453590126241959 ) ) ;
#14800 = VERTEX_POINT ( 'NONE', #17396 ) ;
#14801 = CARTESIAN_POINT ( 'NONE',  ( 1.137810555388867773, -1.046521029022079216E-15, -11.94593600937347055 ) ) ;
#14802 = CARTESIAN_POINT ( 'NONE',  ( -2.842901148319972204, 31.28222014544887486, -13.19749263385335247 ) ) ;
#14803 = CARTESIAN_POINT ( 'NONE',  ( 4.648327100776453946, 73.01265558291817115, -12.67451152641439549 ) ) ;
#14804 = CARTESIAN_POINT ( 'NONE',  ( 7.272992578804308828, -13.02000000000000313, 10.01041549318726709 ) ) ;
#14805 = DIRECTION ( 'NONE',  ( 0.000000000000000000, 0.000000000000000000, -1.000000000000000000 ) ) ;
#14806 = CARTESIAN_POINT ( 'NONE',  ( 10.92172942406179104, -10.27000000000000135, -7.935100905948385908 ) ) ;
#14807 = CARTESIAN_POINT ( 'NONE',  ( -12.81304320705199906, 53.08405703288592292, 4.274644209259282235 ) ) ;
#14808 = CARTESIAN_POINT ( 'NONE',  ( 7.272992578804311492, 49.88000000000000256, -10.01041549318726709 ) ) ;
#14809 = CARTESIAN_POINT ( 'NONE',  ( 4.171729424061789260, 64.82999999999999829, 12.83926296998457417 ) ) ;
#14810 = CARTESIAN_POINT ( 'NONE',  ( 12.52626665340286216, 51.24701910560337836, 5.034456727426829481 ) ) ;
#14811 = CARTESIAN_POINT ( 'NONE',  ( -10.24782649191965334, 37.59234768399701210, -8.788179505534850833 ) ) ;
#14812 = CARTESIAN_POINT ( 'NONE',  ( 6.552616672584657742, 35.92103225518364695, 11.80513931794910576 ) ) ;
#14813 = CARTESIAN_POINT ( 'NONE',  ( -13.16986379959834252, -30.14374999999995097, -13.16986379960055409 ) ) ;
#14814 = EDGE_CURVE ( 'NONE', #3534, #11076, #9141, .T. ) ;
#14815 = CARTESIAN_POINT ( 'NONE',  ( -10.51495019309605716, 74.25306979935668039, 8.466823935618753794 ) ) ;
#14816 = VECTOR ( 'NONE', #17327, 1000.000000000000000 ) ;
#14817 = CARTESIAN_POINT ( 'NONE',  ( -13.30028092895002700, 76.84866536761713007, -2.313556944805478022 ) ) ;
#14818 = CARTESIAN_POINT ( 'NONE',  ( -12.29284966417927016, 80.13423796449390579, 5.580253127422897919 ) ) ;
#14819 = CARTESIAN_POINT ( 'NONE',  ( -5.318689435350380634, 80.93000000000004945, 11.55616787654584421 ) ) ;
#14820 = CARTESIAN_POINT ( 'NONE',  ( -10.92172942406178926, 7.629999999999998117, -7.935100905948389460 ) ) ;
#14821 = CARTESIAN_POINT ( 'NONE',  ( 7.272992578804311492, -0.1199999999999976641, -10.01041549318726709 ) ) ;
#14822 = CARTESIAN_POINT ( 'NONE',  ( 3.636496289402154414, 48.82999999999999829, 11.19198476289190936 ) ) ;
#14823 = CARTESIAN_POINT ( 'NONE',  ( -4.711679271993004292, -55.15312499999986784, -11.37500000000039435 ) ) ;
#14824 = CARTESIAN_POINT ( 'NONE',  ( -18.62500000000000000, -41.62499999999990052, -1.562973063126292555E-12 ) ) ;
#14825 = CARTESIAN_POINT ( 'NONE',  ( -13.49999999999999822, -10.22000000000000419, -4.386415899144240349 ) ) ;
#14826 = CARTESIAN_POINT ( 'NONE',  ( -7.556756315141740288, 40.46334594926985773, -11.19000999533063201 ) ) ;
#14827 = CARTESIAN_POINT ( 'NONE',  ( 10.92172942406179104, 35.72999999999999687, -7.935100905948385908 ) ) ;
#14828 = CARTESIAN_POINT ( 'NONE',  ( 10.30576900039498867, 75.09546229751185820, 8.720167078007317940 ) ) ;
#14829 = DIRECTION ( 'NONE',  ( 0.000000000000000000, -1.000000000000000000, 0.000000000000000000 ) ) ;
#14830 = CARTESIAN_POINT ( 'NONE',  ( -9.520470885617717371, 42.22999999999999687, 6.917026985038133624 ) ) ;
#14831 = CARTESIAN_POINT ( 'NONE',  ( -7.308310390151198987, 41.40732279357077772, 11.35125782457317278 ) ) ;
#14832 = CARTESIAN_POINT ( 'NONE',  ( -5.555424162506318098, 58.38152377935421811, -12.30588174299387028 ) ) ;
#14833 = CARTESIAN_POINT ( 'NONE',  ( 4.940072834807441637, 44.85814714621098886, 12.56428305801228973 ) ) ;
#14834 = DIRECTION ( 'NONE',  ( 0.000000000000000000, 0.000000000000000000, -1.000000000000000000 ) ) ;
#14835 = CARTESIAN_POINT ( 'NONE',  ( 9.651130384012091668, 30.06106401149679641, 9.446356526885642424 ) ) ;
#14836 = CARTESIAN_POINT ( 'NONE',  ( -19.29752010712827826, 5.918584287042170544, -17.42428528562878398 ) ) ;
#14837 = EDGE_CURVE ( 'NONE', #8302, #1729, #6073, .T. ) ;
#14838 = CARTESIAN_POINT ( 'NONE',  ( -5.772320974614566502, 49.38986566563944791, -12.21294285155656034 ) ) ;
#14839 = CARTESIAN_POINT ( 'NONE',  ( 13.36804092920415599, 63.49585643151682746, -1.882948519353985439 ) ) ;
#14840 = CARTESIAN_POINT ( 'NONE',  ( 10.80847967602615078, 42.12344236956776200, 8.090054399549632791 ) ) ;
#14841 = CARTESIAN_POINT ( 'NONE',  ( 2.270588706968536652, 38.76161630363158395, 13.30973914928087254 ) ) ;
#14842 = ORIENTED_EDGE ( 'NONE', *, *, #12057, .T. ) ;
#14843 = CARTESIAN_POINT ( 'NONE',  ( 4.171729424061791924, 75.03000000000000114, -12.83926296998457239 ) ) ;
#14844 = CARTESIAN_POINT ( 'NONE',  ( -4.171729424061791036, 49.53000000000000114, 12.83926296998457239 ) ) ;
#14845 = VECTOR ( 'NONE', #15451, 1000.000000000000000 ) ;
#14846 = CARTESIAN_POINT ( 'NONE',  ( 8.343458848123578520, 17.98000000000000398, 11.48378591275254124 ) ) ;
#14847 = ORIENTED_EDGE ( 'NONE', *, *, #1788, .F. ) ;
#14848 = CARTESIAN_POINT ( 'NONE',  ( -12.69936835568980982, 43.76447789027633917, -4.580193949658626806 ) ) ;
#14849 = CARTESIAN_POINT ( 'NONE',  ( -13.16986379959834252, -56.19374999999985931, -13.16986379960055054 ) ) ;
#14850 = CARTESIAN_POINT ( 'NONE',  ( 12.98358486008634394, 60.56220495594141795, -3.698251661676718705 ) ) ;
#14851 = CARTESIAN_POINT ( 'NONE',  ( -4.171729424061791036, 12.53000000000001357, 12.83926296998457239 ) ) ;
#14852 = CARTESIAN_POINT ( 'NONE',  ( 12.33294000059855122, 57.63073804451487803, -5.490917873338714728 ) ) ;
#14853 = CARTESIAN_POINT ( 'NONE',  ( 9.520470885617715595, 70.12999999999999545, 6.917026985038134512 ) ) ;
#14854 = CARTESIAN_POINT ( 'NONE',  ( -11.76794919243112325, 80.78000000000000114, -3.823638476888998827 ) ) ;
#14855 = CARTESIAN_POINT ( 'NONE',  ( -10.16915865940034536, 47.27191544427423509, 8.882609797670191654 ) ) ;
#14856 = CARTESIAN_POINT ( 'NONE',  ( 8.464728390624178894E-06, 46.17999963826949994, -13.49999999999734790 ) ) ;
#14857 = DIRECTION ( 'NONE',  ( 0.000000000000000000, 0.000000000000000000, 1.000000000000000000 ) ) ;
#14858 = CARTESIAN_POINT ( 'NONE',  ( 13.50000000000000000, 38.42999999999999972, 1.653273178848926867E-15 ) ) ;
#14859 = CARTESIAN_POINT ( 'NONE',  ( -6.935444911370063359, 9.999999999999992895, -10.66458871277817622 ) ) ;
#14860 = CARTESIAN_POINT ( 'NONE',  ( -8.043339635996302306, -72.84374999999981526, -8.043339635997654113 ) ) ;
#14861 = ADVANCED_FACE ( 'NONE', ( #3025 ), #220, .F. ) ;
#14862 = CARTESIAN_POINT ( 'NONE',  ( -8.697098998243532012E-15, 64.18000000000002103, -13.50000000000000000 ) ) ;
#14863 = CARTESIAN_POINT ( 'NONE',  ( 13.49437229710556529, 33.44374862988300379, -0.4003926536058359242 ) ) ;
#14864 = CARTESIAN_POINT ( 'NONE',  ( -9.875337133188997640, 73.57270964355765841, -9.205946121983142660 ) ) ;
#14865 = CARTESIAN_POINT ( 'NONE',  ( -8.050004039213265017, 7.892626838387373667, -16.80522879631183031 ) ) ;
#14866 = ORIENTED_EDGE ( 'NONE', *, *, #1031, .F. ) ;
#14867 = CARTESIAN_POINT ( 'NONE',  ( -13.50000000000000000, 42.92999999999999261, -3.306546357697853733E-15 ) ) ;
#14868 = VERTEX_POINT ( 'NONE', #13980 ) ;
#14869 = CARTESIAN_POINT ( 'NONE',  ( 4.711679271993006957, -54.07812499999989342, 11.37500000000039257 ) ) ;
#14870 = CARTESIAN_POINT ( 'NONE',  ( -11.18637559572935380, 44.21414602053655329, 7.557466717348048313 ) ) ;
#14871 = CARTESIAN_POINT ( 'NONE',  ( -7.499999999999997335, -25.28130420966591174, -8.086389325435080266 ) ) ;
#14872 = CARTESIAN_POINT ( 'NONE',  ( -13.50000000000000000, 43.92999999999999972, -3.306546357697853733E-15 ) ) ;
#14873 = CARTESIAN_POINT ( 'NONE',  ( -13.50000000000000000, 45.92999999999999972, -3.306546357697853733E-15 ) ) ;
#14874 = CARTESIAN_POINT ( 'NONE',  ( -12.92930772591764210, 71.06914952832075016, 3.883688861026760364 ) ) ;
#14875 = EDGE_CURVE ( 'NONE', #3274, #1725, #11268, .T. ) ;
#14876 = CARTESIAN_POINT ( 'NONE',  ( -13.16986379960055409, -36.45624999999989768, 13.16986379959834252 ) ) ;
#14877 = CARTESIAN_POINT ( 'NONE',  ( -12.82678188565936317, 68.08144701978382329, 4.209989458535909002 ) ) ;
#14878 = CARTESIAN_POINT ( 'NONE',  ( 18.62500000000064659, -27.09062499999992113, -7.714727599197336083 ) ) ;
#14879 = CARTESIAN_POINT ( 'NONE',  ( 13.49914950589871232, 54.43523986101267553, -0.1529510493150832429 ) ) ;
#14880 = B_SPLINE_CURVE_WITH_KNOTS ( 'NONE', 3,
 ( #5764, #9660, #7088, #8595, #531, #8421, #272, #13774, #12642, #12730, #16435, #8682, #8511, #12471, #1588, #13948, #358, #4337, #4517, #5682, #9747, #7005, #15091, #15359, #2990, #1844, #11148, #16523, #4430, #1762, #5940, #11320, #15184, #3264, #618, #3085, #16699, #4604, #7172, #6029, #16342, #12560, #445, #5856, #9924, #4251, #2357, #6197, #1047, #6371, #7439, #3442, #870, #9025, #10096, #4691, #15446, #12987, #11754, #3355, #16872, #4777, #12818, #2183, #10180, #705, #2096, #6115, #17131, #11496, #14380, #6281, #7522, #8771, #14126, #2270, #9119, #13160, #14297, #14211, #15531, #2012, #10264, #11669, #15615, #8857, #787, #7611, #15796, #17044, #4949, #12903, #3524, #959, #7696, #11583, #8938, #16958, #4861, #10352, #3611, #7790, #15706, #13073, #5040, #11412, #10438, #3702, #16784, #14468, #2531, #11845, #6716, #9204, #7959, #17220, #10521, #14810, #4138, #8226, #9377, #5130, #9551, #14555, #5308, #12094, #10690, #1135, #13329, #14726, #10860, #13411, #17476, #11925, #16057, #13498, #9461, #7870, #3964, #5218, #2439, #2614, #15972, #2795, #3875, #2704, #17392, #13587, #16139, #5389, #15884, #10605, #1220, #3791, #10774, #13248, #4049, #9290, #1301, #8044, #8134, #6546, #1389, #17306, #6804, #6459, #14643, #6632, #12012, #12182, #73, #5479, #16229, #14901, #16414, #9904, #9992, #1566, #11300, #11129, #4316, #15339, #12623, #426, #9640, #8663, #11042, #5832 ),
 .UNSPECIFIED., .F., .F.,
 ( 4, 2, 2, 2, 2, 2, 2, 2, 2, 1, 1, 2, 2, 2, 2, 2, 2, 2, 2, 2, 2, 1, 1, 1, 1, 2, 2, 2, 1, 2, 2, 1, 2, 2, 2, 1, 2, 2, 1, 1, 2, 2, 2, 2, 1, 1, 1, 2, 2, 1, 2, 2, 1, 1, 2, 2, 2, 2, 2, 1, 2, 2, 2, 2, 2, 2, 2, 1, 1, 1, 1, 2, 2, 1, 2, 2, 1, 2, 2, 1, 1, 2, 2, 2, 2, 2, 2, 1, 2, 2, 2, 2, 2, 1, 1, 1, 1, 1, 1, 1, 1, 1, 2, 2, 2, 2, 2, 1, 1, 2, 2, 1, 1, 4 ),
 ( 0.5637389225892408540, 0.5641984839263527451, 0.5644282645949086907, 0.5646580452634646363, 0.5655771679376883077, 0.5664962906119120900, 0.5669558519490238702, 0.5670707422833018985, 0.5670994648668713500, 0.5671281874504409126, 0.5671856326175798158, 0.5674154132861357613, 0.5683345359603594327, 0.5692536586345832150, 0.5694834393031390496, 0.5697132199716949952, 0.5701727813088068864, 0.5710919039830305577, 0.5715514653201424489, 0.5715801879037119004, 0.5715945491954966817, 0.5716089104872814630, 0.5716663556544203662, 0.5717812459886983945, 0.5720110266572544511, 0.5724705879943665643, 0.5729301493314785665, 0.5733897106685906797, 0.5735046010028687080, 0.5735620461700077222, 0.5735907687535771737, 0.5736194913371466253, 0.5738492720057026819, 0.5747683946799269084, 0.5749981753484828539, 0.5750556205156218681, 0.5750843430991914307, 0.5750915237450837658, 0.5750987043909762120, 0.5751130656827608822, 0.5752279560170389106, 0.5756875173541509128, 0.5761470786912630260, 0.5763768593598190826, 0.5764917496940969999, 0.5765491948612360140, 0.5765779174448055766, 0.5765850980906979117, 0.5765922787365902469, 0.5766066400283750282, 0.5775257627025992546, 0.5779853240397113678, 0.5780427692068503820, 0.5780714917904198336, 0.5780858530822046149, 0.5781002143739893961, 0.5782151047082674244, 0.5784448853768234811, 0.5793640080510475965, 0.5794788983853256248, 0.5795363435524646389, 0.5795937887196036531, 0.5798235693881597097, 0.5802831307252717119, 0.5812022533994959383, 0.5816618147366079405, 0.5818915954051639972, 0.5820064857394420255, 0.5820639309065810396, 0.5820782921983658209, 0.5820854728442581560, 0.5820890631672043236, 0.5820926534901504912, 0.5821213760737200538, 0.5839596214221685067, 0.5844191827592806199, 0.5845340730935586482, 0.5845915182606976623, 0.5846058795524824436, 0.5846202408442672249, 0.5846489634278366765, 0.5848787440963928441, 0.5857978667706170706, 0.5867169894448414080, 0.5869467701133974646, 0.5870616604476754929, 0.5871191056148145071, 0.5871765507819535213, 0.5876361121190656345, 0.5885552347932898609, 0.5894743574675140874, 0.5895892478017921157, 0.5896036090935768970, 0.5896179703853616783, 0.5896466929689311298, 0.5897041381360701440, 0.5899339188046262006, 0.5903934801417383138, 0.5906232608102943704, 0.5907381511445723987, 0.5907955963117114129, 0.5908243188952809755, 0.5908386801870656457, 0.5908530414788504270, 0.5913126028159625402, 0.5917721641530746535, 0.5920019448216307101, 0.5920593899887697242, 0.5920881125723392868, 0.5920952932182316220, 0.5921024738641239571, 0.5921168351559087384, 0.5922317254901867667, 0.5931508481644109931 ),
 .UNSPECIFIED. ) ;
#14881 = CARTESIAN_POINT ( 'NONE',  ( 18.62500000000064304, -84.29062499999983515, -7.714727599197335195 ) ) ;
#14882 = CARTESIAN_POINT ( 'NONE',  ( -11.88051552057379645, 64.69276546394441141, -6.411193178701971362 ) ) ;
#14883 = VERTEX_POINT ( 'NONE', #12508 ) ;
#14884 = CARTESIAN_POINT ( 'NONE',  ( -9.520470885617715595, 21.63000000000000966, -6.917026985038136289 ) ) ;
#14885 = CARTESIAN_POINT ( 'NONE',  ( -13.49999999999999822, 63.78000000000000114, -4.386415899144240349 ) ) ;
#14886 = CARTESIAN_POINT ( 'NONE',  ( -11.62103019124827696, 35.18589392510355651, 6.873052513693640897 ) ) ;
#14887 = CIRCLE ( 'NONE', #2200, 9.000000000000000000 ) ;
#14888 = VERTEX_POINT ( 'NONE', #1709 ) ;
#14889 = CARTESIAN_POINT ( 'NONE',  ( 12.99172110702898841, 78.56117060242844730, -3.670802009133220078 ) ) ;
#14890 = CARTESIAN_POINT ( 'NONE',  ( -9.840429937218175382, -2.585303254002297467E-15, -8.208115554517609880 ) ) ;
#14891 = CARTESIAN_POINT ( 'NONE',  ( -10.37153830093552820, 31.59880329612760264, -8.642521494078742705 ) ) ;
#14892 = CARTESIAN_POINT ( 'NONE',  ( 8.321323615989754785, 72.86260839518769217, -10.63042200351674182 ) ) ;
#14893 = CARTESIAN_POINT ( 'NONE',  ( -3.636496289402156190, -7.469999999999997087, 11.19198476289190758 ) ) ;
#14894 = CARTESIAN_POINT ( 'NONE',  ( 0.1284016000230580046, 79.17538378579617131, -13.49947537073678916 ) ) ;
#14895 = CARTESIAN_POINT ( 'NONE',  ( -10.92172942406179104, -17.76999999999999957, 7.935100905948385908 ) ) ;
#14896 = CARTESIAN_POINT ( 'NONE',  ( 4.171729424061791924, 76.03000000000000114, -12.83926296998457239 ) ) ;
#14897 = CARTESIAN_POINT ( 'NONE',  ( -13.47435762513628887, 52.95904153983646978, 0.8409795588075931194 ) ) ;
#14898 = EDGE_CURVE ( 'NONE', #17257, #12765, #3293, .T. ) ;
#14899 = CARTESIAN_POINT ( 'NONE',  ( 11.76794919243112325, 46.27999999999999403, 3.823638476888996607 ) ) ;
#14900 = CARTESIAN_POINT ( 'NONE',  ( -8.343458848123576743, 63.48000000000001108, -11.48378591275254301 ) ) ;
#14901 = CARTESIAN_POINT ( 'NONE',  ( 2.659296992907285606, 50.77569272368128139, 13.23688342416419061 ) ) ;
#14902 = CARTESIAN_POINT ( 'NONE',  ( -5.978783164607675005, 37.39809822006411366, -12.10535056917534114 ) ) ;
#14903 = CARTESIAN_POINT ( 'NONE',  ( 13.30492957411319210, 36.34963648306288775, 2.286669702493058676 ) ) ;
#14904 = CARTESIAN_POINT ( 'NONE',  ( 13.16986379959833897, -38.46874999999992895, 13.16986379960055409 ) ) ;
#14905 = CARTESIAN_POINT ( 'NONE',  ( -8.458738825805157902, 74.35630711111390667, 10.52140770450354168 ) ) ;
#14906 = CARTESIAN_POINT ( 'NONE',  ( -13.49239393192323533, 76.94558248929156719, 0.4532043396295901694 ) ) ;
#14907 = CARTESIAN_POINT ( 'NONE',  ( -9.393480485980296280, 80.31162245988731740, 9.698493905942369153 ) ) ;
#14908 = CARTESIAN_POINT ( 'NONE',  ( -21.14483242576217847, 7.170662809914417402, 2.970370385949070435 ) ) ;
#14909 = CARTESIAN_POINT ( 'NONE',  ( 13.49999999999999822, 4.280000000000002025, 4.386415899144236796 ) ) ;
#14910 = CYLINDRICAL_SURFACE ( 'NONE', #15666, 13.50000000000000000 ) ;
#14911 = CARTESIAN_POINT ( 'NONE',  ( 9.520470885617715595, -0.8699999999999957767, 6.917026985038135400 ) ) ;
#14912 = CARTESIAN_POINT ( 'NONE',  ( 11.76794919243112680, 43.57999999999999119, -3.823638476888993942 ) ) ;
#14913 = CARTESIAN_POINT ( 'NONE',  ( 13.16986379960055054, -2.081249999999994937, -13.16986379959834430 ) ) ;
#14914 = CARTESIAN_POINT ( 'NONE',  ( -13.50000000000000000, -13.06999999999999851, -3.469446951953614189E-15 ) ) ;
#14915 = CARTESIAN_POINT ( 'NONE',  ( -10.23470376096455858, 40.59170058523897495, -8.803567802926888675 ) ) ;
#14916 = FACE_OUTER_BOUND ( 'NONE', #16533, .T. ) ;
#14917 = CARTESIAN_POINT ( 'NONE',  ( 10.28800811278561511, 75.09451940748620302, 8.741114209820295855 ) ) ;
#14918 = CIRCLE ( 'NONE', #7328, 6.000000000000001776 ) ;
#14919 = CARTESIAN_POINT ( 'NONE',  ( 5.796175271902052728, -7.251940901129036557E-16, -15.63158725347429545 ) ) ;
#14920 = CARTESIAN_POINT ( 'NONE',  ( 11.76794919243112325, 34.42999999999999261, 1.441158131103945434E-15 ) ) ;
#14921 = CARTESIAN_POINT ( 'NONE',  ( 6.616676866212972294E-07, 41.68001839382905160, 13.49999999999996625 ) ) ;
#14922 = CARTESIAN_POINT ( 'NONE',  ( -4.021251358392601283, 58.32458930914320661, -12.88728184459310278 ) ) ;
#14923 = CARTESIAN_POINT ( 'NONE',  ( 0.000000000000000000, 108.9300000000000068, 0.000000000000000000 ) ) ;
#14924 = B_SPLINE_CURVE_WITH_KNOTS ( 'NONE', 3,
 ( #964, #11588, #2101, #2275, #11931, #17136, #4866, #7528, #15712, #17311, #9210, #14474, #6202, #5225, #7616, #2362, #12909, #13078, #16964, #15537, #2445, #4955, #8944, #14386, #6551, #14216, #5046, #10269, #792, #10358, #7876, #3707, #14302, #9124, #6377, #15803, #15621, #7701, #2189, #3616, #13166, #9032, #14561, #12993, #3447, #875, #6286, #11674, #13253, #11761, #10443, #1140, #1053, #6465, #11850, #17225, #15889, #5136, #10526, #8864, #3798, #5313, #5579, #6638, #8231, #79, #6721, #9297, #14731, #10696, #2620, #13675, #10960, #2888, #14906, #13592, #8320, #7964, #3880, #6903, #16062, #16328, #12366, #5484, #10866, #3970, #14817, #173, #1486, #12018, #8139, #9382, #13334, #8053, #2800, #1573, #4054, #9556, #13418, #260, #16144, #12277, #15977, #1307, #12099, #14648, #16235, #1226, #4236, #17481, #4143, #9468, #13504, #17397, #2536, #2710, #6991, #5395, #6810, #10780, #1394, #12187, #9646, #10610, #14996, #16684, #3070, #14027, #14115, #5752, #15078, #2978, #12807, #8671, #12546, #11048, #8408, #7427, #4591, #9732, #1916, #2001, #11136, #1828, #13760, #16597, #1660, #343, #6016, #5668, #7075, #16420, #4323, #11399, #12459, #7245, #16509, #4415, #5840, #9825, #16771, #15170, #5927, #8496, #13847, #1749, #7335, #4504, #9998, #4679, #7161, #433, #11222, #9911, #15258, #3156, #12630 ),
 .UNSPECIFIED., .F., .F.,
 ( 4, 2, 2, 2, 1, 1, 2, 2, 1, 2, 2, 2, 2, 2, 1, 1, 1, 1, 2, 2, 2, 2, 1, 2, 2, 1, 1, 2, 2, 2, 2, 1, 2, 2, 1, 1, 2, 2, 2, 2, 2, 2, 1, 2, 2, 1, 1, 2, 2, 2, 2, 2, 2, 1, 1, 2, 2, 2, 2, 2, 2, 2, 1, 2, 2, 2, 2, 1, 1, 1, 2, 2, 2, 1, 2, 2, 1, 1, 2, 2, 2, 2, 2, 2, 1, 1, 2, 2, 2, 1, 1, 2, 2, 1, 2, 2, 2, 1, 2, 2, 1, 1, 2, 2, 4 ),
 ( 0.06374556628509139844, 0.06466468642086431462, 0.06558380655663724468, 0.06604336662452370277, 0.06627314665846693875, 0.06638803667543854981, 0.06640239792756000292, 0.06641675917968145604, 0.06644548168392436227, 0.06650292669241016086, 0.06742204682818311867, 0.06834116696395607649, 0.06835552821607752960, 0.06836988946819898272, 0.06839861197244188895, 0.06845605698092770142, 0.06857094699789934023, 0.06880072703184259009, 0.06926028709972911757, 0.07017940723550215865, 0.07109852737127521360, 0.07201764750704825468, 0.07224742754099151842, 0.07226178879311297154, 0.07227615004523442466, 0.07230487254947733089, 0.07236231755796314336, 0.07247720757493476829, 0.07293676764282128189, 0.07385588777859430909, 0.07408566781253757283, 0.07420055782950919776, 0.07421491908163066475, 0.07422928033375211787, 0.07425800283799502410, 0.07431544784648083657, 0.07477500791436741956, 0.07569412805014058554, 0.07615368811802715465, 0.07661324818591373764, 0.07753236832168688974, 0.07799192838957347274, 0.07810681840654511154, 0.07812117965866657854, 0.07813554091078803165, 0.07816426341503093789, 0.07822170842351676423, 0.07845148845746005573, 0.07937060859323322171, 0.07983016866111980470, 0.08005994869506309619, 0.08007430994718454931, 0.08008867119930601630, 0.08011739370354893641, 0.08017483871203481827, 0.08028972872900659585, 0.08120884886478078879, 0.08166840893266788526, 0.08189818896661142655, 0.08201307898358320414, 0.08202744023570467113, 0.08204180148782613813, 0.08207052399206908599, 0.08212796900055498173, 0.08396620927210349250, 0.08398057052422497337, 0.08399493177634644037, 0.08402365428058938823, 0.08408109928907527009, 0.08419598930604704767, 0.08442576933999061672, 0.08488532940787774095, 0.08580444954365200327, 0.08591933956062379474, 0.08593370081274526173, 0.08594806206486674260, 0.08597678456910966271, 0.08603422957759551681, 0.08626400961153887770, 0.08672356967942559947, 0.08764268981519902912, 0.08787246984914237613, 0.08788683110126384312, 0.08790119235338529624, 0.08792991485762821635, 0.08798735986611404269, 0.08810224988308569538, 0.08856180995097232000, 0.08948093008674556925, 0.08971071012068887462, 0.08982560013766054119, 0.08983996138978199431, 0.08985432264190344742, 0.08988304514614636753, 0.08994049015463219388, 0.09040005022251877687, 0.09131917035829195672, 0.09143406037526360941, 0.09149150538374943575, 0.09150586663587088887, 0.09152022788799234199, 0.09154895039223526210, 0.09177873042617858135, 0.09223829049406520597, 0.09315741062983846910 ),
 .UNSPECIFIED. ) ;
#14925 = CARTESIAN_POINT ( 'NONE',  ( -2.138189944381240881, 55.60311857767972299, 13.49999999999999822 ) ) ;
#14926 = FACE_OUTER_BOUND ( 'NONE', #11012, .T. ) ;
#14927 = AXIS2_PLACEMENT_3D ( 'NONE', #10380, #3472, #11525 ) ;
#14928 = CARTESIAN_POINT ( 'NONE',  ( -8.891200544363830713E-16, 58.67999999999999261, 13.50000000000000000 ) ) ;
#14929 = CARTESIAN_POINT ( 'NONE',  ( -10.11724169932725914, 49.58540793223827592, -8.938216045275497734 ) ) ;
#14930 = CARTESIAN_POINT ( 'NONE',  ( 12.88992561142933191, 63.28600745562859231, 4.012516480704441335 ) ) ;
#14931 = CARTESIAN_POINT ( 'NONE',  ( 10.61024901455322578, 42.11222895898699647, 8.347195607159086705 ) ) ;
#14932 = CARTESIAN_POINT ( 'NONE',  ( 4.325464046711072541, 38.83554751821355211, 12.78834246629441473 ) ) ;
#14933 = ORIENTED_EDGE ( 'NONE', *, *, #16812, .F. ) ;
#14934 = CARTESIAN_POINT ( 'NONE',  ( -12.00000000000000178, 3.796025403784440311, -2.718289652585035561E-15 ) ) ;
#14935 = FACE_BOUND ( 'NONE', #12422, .T. ) ;
#14936 = CARTESIAN_POINT ( 'NONE',  ( -13.50000000000000000, 13.92999999999999794, -3.469446951953614189E-15 ) ) ;
#14937 = ORIENTED_EDGE ( 'NONE', *, *, #10645, .F. ) ;
#14938 = CARTESIAN_POINT ( 'NONE',  ( -8.694518465881534652, 43.51465161020028205, -10.32740934920959930 ) ) ;
#14939 = CARTESIAN_POINT ( 'NONE',  ( -7.500000000000001776, 104.9408589258552666, -8.949127168380913488 ) ) ;
#14940 = CARTESIAN_POINT ( 'NONE',  ( 12.68261237030094613, 60.59908932111539315, -4.680264340947544177 ) ) ;
#14941 = PRODUCT_DEFINITION_SHAPE ( 'NONE', 'NONE',  #17490 ) ;
#14942 = CARTESIAN_POINT ( 'NONE',  ( -13.49999999999999822, 9.079999999999996518, 4.386415899144235908 ) ) ;
#14943 = DIRECTION ( 'NONE',  ( 0.000000000000000000, 0.000000000000000000, -1.000000000000000000 ) ) ;
#14944 = CARTESIAN_POINT ( 'NONE',  ( 12.68202363619548656, 66.59736773260050313, -4.628554097373979381 ) ) ;
#14945 = CARTESIAN_POINT ( 'NONE',  ( 3.243294801669318606, 56.79662143353648673, 13.10462081408920909 ) ) ;
#14946 = EDGE_CURVE ( 'NONE', #17169, #2565, #5852, .T. ) ;
#14947 = CARTESIAN_POINT ( 'NONE',  ( 3.636496289402157078, 56.02999999999999403, -11.19198476289190936 ) ) ;
#14948 = CARTESIAN_POINT ( 'NONE',  ( -7.272992578804307939, 68.48000000000000398, -10.01041549318726886 ) ) ;
#14949 = CARTESIAN_POINT ( 'NONE',  ( -3.572130815311478358, 47.55156684393307387, 13.01911799694966554 ) ) ;
#14950 = CARTESIAN_POINT ( 'NONE',  ( 5.547257296411079786, 45.97874116037399261, -12.30763780998237067 ) ) ;
#14951 = LINE ( 'NONE', #9600, #13600 ) ;
#14952 = FACE_OUTER_BOUND ( 'NONE', #5276, .T. ) ;
#14953 = CARTESIAN_POINT ( 'NONE',  ( 2.785878927130813844E-06, 56.68007738487546732, 13.49999999999942979 ) ) ;
#14954 = CARTESIAN_POINT ( 'NONE',  ( 8.043339635997654113, -52.03124999999987921, -8.043339635996304082 ) ) ;
#14955 = CARTESIAN_POINT ( 'NONE',  ( -13.50000000000000000, 39.92999999999999972, -3.306546357697853733E-15 ) ) ;
#14956 = CARTESIAN_POINT ( 'NONE',  ( 4.711679271993006068, -46.82812499999989342, 11.37500000000039257 ) ) ;
#14957 = CARTESIAN_POINT ( 'NONE',  ( 11.98594149431912648, 33.65924774496181726, -6.211891203905776315 ) ) ;
#14958 = DIRECTION ( 'NONE',  ( 0.000000000000000000, 1.000000000000000000, 0.000000000000000000 ) ) ;
#14959 = CARTESIAN_POINT ( 'NONE',  ( -9.111282024567884719, 8.062232123460391975, -15.52398764842096845 ) ) ;
#14960 = VERTEX_POINT ( 'NONE', #11183 ) ;
#14961 = CARTESIAN_POINT ( 'NONE',  ( 2.445080149700053643E-15, 42.17999999999999261, -13.50000000000000000 ) ) ;
#14962 = CARTESIAN_POINT ( 'NONE',  ( -13.49644181220360650, 40.94171918537661981, 0.3420769386924029098 ) ) ;
#14963 = CARTESIAN_POINT ( 'NONE',  ( -18.62500000000000000, -32.22499999999993747, -1.562973063126292757E-12 ) ) ;
#14964 = CARTESIAN_POINT ( 'NONE',  ( -13.47468169643279801, 43.95856576188575815, 0.8271159465435392599 ) ) ;
#14965 = CARTESIAN_POINT ( 'NONE',  ( 13.50000000000000355, 16.58000000000000185, -4.386415899144233244 ) ) ;
#14966 = CARTESIAN_POINT ( 'NONE',  ( -8.704847339800608097, 8.055054264001460851, 15.78643792884161456 ) ) ;
#14967 = CARTESIAN_POINT ( 'NONE',  ( 2.607531440858944223E-15, 46.17999999999999261, -14.19474002721660355 ) ) ;
#14968 = CARTESIAN_POINT ( 'NONE',  ( -10.92172942406179104, 49.23000000000000398, 7.935100905948387684 ) ) ;
#14969 = CARTESIAN_POINT ( 'NONE',  ( -13.49727400116812426, 70.92069023477120027, -0.2713576259430695581 ) ) ;
#14970 = EDGE_CURVE ( 'NONE', #11029, #14800, #4465, .T. ) ;
#14971 = CARTESIAN_POINT ( 'NONE',  ( -13.16986379959834252, -48.94374999999985931, -13.16986379960055409 ) ) ;
#14972 = CARTESIAN_POINT ( 'NONE',  ( -10.98011399424891366, 67.63341784965055581, -7.854123836487283405 ) ) ;
#14973 = CARTESIAN_POINT ( 'NONE',  ( -13.16986379959834252, -65.59374999999981526, -13.16986379960055409 ) ) ;
#14974 = CARTESIAN_POINT ( 'NONE',  ( 13.10268814798864234, 54.54569041227427562, -3.253754133682983607 ) ) ;
#14975 = CARTESIAN_POINT ( 'NONE',  ( -12.73420858044403836, 65.09178978912700586, 4.482361047366480555 ) ) ;
#14976 = ORIENTED_EDGE ( 'NONE', *, *, #14814, .F. ) ;
#14977 = CARTESIAN_POINT ( 'NONE',  ( -13.47034220899966961, 34.89910285180874183, -0.8944510538467952410 ) ) ;
#14978 = ORIENTED_EDGE ( 'NONE', *, *, #13148, .F. ) ;
#14979 = CARTESIAN_POINT ( 'NONE',  ( 13.01895187323182412, 78.55753440904214813, -3.573211116871425119 ) ) ;
#14980 = CARTESIAN_POINT ( 'NONE',  ( 2.138189944381238661, 49.75688142232025513, 13.50000000000000000 ) ) ;
#14981 = CARTESIAN_POINT ( 'NONE',  ( -5.579618841234667670, 31.38249916496278757, -12.29310188421200678 ) ) ;
#14982 = CARTESIAN_POINT ( 'NONE',  ( 9.978235625303845779, 72.78197465687738088, -9.095030402899643818 ) ) ;
#14983 = CARTESIAN_POINT ( 'NONE',  ( -1.328659818498353332E-07, 59.67999629905246195, 13.49999999999999822 ) ) ;
#14984 = CARTESIAN_POINT ( 'NONE',  ( -13.50000000000000000, -12.06999999999999673, -3.469446951953614189E-15 ) ) ;
#14985 = CARTESIAN_POINT ( 'NONE',  ( -13.49999999999999822, 74.08000000000001251, 4.386415899144235908 ) ) ;
#14986 = CARTESIAN_POINT ( 'NONE',  ( -13.38626367270875761, 52.99368492772342165, 1.826722430351332305 ) ) ;
#14987 = EDGE_CURVE ( 'NONE', #2562, #1172, #8366, .T. ) ;
#14988 = CARTESIAN_POINT ( 'NONE',  ( -9.520470885617715595, 44.62999999999999545, -6.917026985038136289 ) ) ;
#14989 = CARTESIAN_POINT ( 'NONE',  ( -10.92172942406178926, 63.63000000000000256, -7.935100905948389460 ) ) ;
#14990 = DIRECTION ( 'NONE',  ( -1.000000000000000000, 0.000000000000000000, -1.075706766891313654E-14 ) ) ;
#14991 = CARTESIAN_POINT ( 'NONE',  ( 12.00929620591970526, 69.20223501009333233, 6.176927723990055519 ) ) ;
#14992 = DIRECTION ( 'NONE',  ( 0.000000000000000000, 0.000000000000000000, 1.000000000000000000 ) ) ;
#14993 = CARTESIAN_POINT ( 'NONE',  ( -2.138189944381243102, 78.25688142232027644, -13.50000000000000000 ) ) ;
#14994 = CARTESIAN_POINT ( 'NONE',  ( -11.37499999999960210, -97.78437499999979821, -4.711679271994911211 ) ) ;
#14995 = CARTESIAN_POINT ( 'NONE',  ( -11.28078867911932370, 74.20825143659133971, 7.415781942181430608 ) ) ;
#14996 = CARTESIAN_POINT ( 'NONE',  ( -9.449293760640395945, 76.55109966697389723, -9.641680980241128296 ) ) ;
#14997 = CARTESIAN_POINT ( 'NONE',  ( 6.123233995736765296E-16, 0.000000000000000000, -5.000000000000000000 ) ) ;
#14998 = CARTESIAN_POINT ( 'NONE',  ( -25.42428528562849266, 0.000000000000000000, -5.441113646577748320 ) ) ;
#14999 = DIRECTION ( 'NONE',  ( -0.000000000000000000, 1.000000000000000000, -0.000000000000000000 ) ) ;
#15000 = CARTESIAN_POINT ( 'NONE',  ( -11.76794919243112325, -7.919999999999998153, 3.823638476888994386 ) ) ;
#15001 = CARTESIAN_POINT ( 'NONE',  ( 7.272992578804308828, 42.97999999999998977, 10.01041549318726886 ) ) ;
#15002 = CARTESIAN_POINT ( 'NONE',  ( 4.171729424061791924, -13.96999999999999709, -12.83926296998457239 ) ) ;
#15003 = CARTESIAN_POINT ( 'NONE',  ( -10.08254685910888249, 40.58366014780975917, -8.978105075904496246 ) ) ;
#15004 = VECTOR ( 'NONE', #15299, 1000.000000000000000 ) ;
#15005 = CARTESIAN_POINT ( 'NONE',  ( -1.328658795546723038E-07, 9.679996299052479714, 13.49999999999999822 ) ) ;
#15006 = CARTESIAN_POINT ( 'NONE',  ( 13.36046613123341054, 75.36200234952120525, 1.941819533583398094 ) ) ;
#15007 = CARTESIAN_POINT ( 'NONE',  ( 4.958022057362319046, -6.117673133592627308E-13, -12.22358761560111695 ) ) ;
#15008 =( LENGTH_UNIT ( ) NAMED_UNIT ( * ) SI_UNIT ( .MILLI., .METRE. ) );
#15009 = DIRECTION ( 'NONE',  ( 0.000000000000000000, 0.000000000000000000, -1.000000000000000000 ) ) ;
#15010 = CARTESIAN_POINT ( 'NONE',  ( -1.097433972752848597, 58.21943276801300726, -13.46203577575871257 ) ) ;
#15011 = CARTESIAN_POINT ( 'NONE',  ( 3.845940030877601057, 44.81806629663489616, 12.94543018042384652 ) ) ;
#15012 = AXIS2_PLACEMENT_3D ( 'NONE', #17484, #13849, #5671 ) ;
#15013 = CARTESIAN_POINT ( 'NONE',  ( 13.49999999999999822, 59.27999999999999403, 4.386415899144236796 ) ) ;
#15014 = DIRECTION ( 'NONE',  ( 0.000000000000000000, 0.000000000000000000, -1.000000000000000000 ) ) ;
#15015 = CARTESIAN_POINT ( 'NONE',  ( 1.102182119232618108E-15, -28.00000000000000000, 6.000000000000001776 ) ) ;
#15016 = CARTESIAN_POINT ( 'NONE',  ( -6.953647091445300354, 49.43771701599564494, -11.57208863864802595 ) ) ;
#15017 = CARTESIAN_POINT ( 'NONE',  ( 11.46408888769126477, 63.16362770892857981, 7.129672723819229674 ) ) ;
#15018 = CARTESIAN_POINT ( 'NONE',  ( 8.623685178462253020, 42.01131593190542191, 10.38745792132406898 ) ) ;
#15019 = CARTESIAN_POINT ( 'NONE',  ( 5.928360391604972968, 48.96387440575580285, -12.12866813512049902 ) ) ;
#15020 = ORIENTED_EDGE ( 'NONE', *, *, #2426, .T. ) ;
#15021 = CARTESIAN_POINT ( 'NONE',  ( -11.76794919243112325, 80.92999999999767624, -5.919446256302011733E-11 ) ) ;
#15022 = CARTESIAN_POINT ( 'NONE',  ( 0.000000000000000000, -28.00000000000000000, 0.000000000000000000 ) ) ;
#15023 = CARTESIAN_POINT ( 'NONE',  ( -13.50000000000000000, 48.92999999999999972, -3.306546357697853733E-15 ) ) ;
#15024 = ORIENTED_EDGE ( 'NONE', *, *, #11447, .F. ) ;
#15025 = CARTESIAN_POINT ( 'NONE',  ( -10.52241331024074356, 43.60707797551511788, -8.460377887765865523 ) ) ;
#15026 = CARTESIAN_POINT ( 'NONE',  ( -7.499999999999998224, 106.7538932235142823, -7.532295102519077190 ) ) ;
#15027 = CARTESIAN_POINT ( 'NONE',  ( 5.354359914900771678, 60.98636505280213527, -12.39747404020963550 ) ) ;
#15028 = CARTESIAN_POINT ( 'NONE',  ( -8.549982208541774191E-16, 15.68000000000000682, 14.19474002721660355 ) ) ;
#15029 = VECTOR ( 'NONE', #5406, 1000.000000000000000 ) ;
#15030 = CARTESIAN_POINT ( 'NONE',  ( 13.45032318530042126, 66.38986098046753170, 1.157148491779020238 ) ) ;
#15031 = CARTESIAN_POINT ( 'NONE',  ( 11.54394565333526401, 57.16869923784576457, 7.014965779171773441 ) ) ;
#15032 = CARTESIAN_POINT ( 'NONE',  ( 7.272992578804311492, 61.87999999999999545, -10.01041549318726709 ) ) ;
#15033 = CARTESIAN_POINT ( 'NONE',  ( 2.607531440858944223E-15, 36.17999999999999972, -14.19474002721660355 ) ) ;
#15034 = CARTESIAN_POINT ( 'NONE',  ( -9.520470885617717371, 69.23000000000000398, 6.917026985038133624 ) ) ;
#15035 = CARTESIAN_POINT ( 'NONE',  ( -10.75877101843568795, 47.23955598554530866, 8.166359762435629221 ) ) ;
#15036 = DIRECTION ( 'NONE',  ( 0.000000000000000000, 0.000000000000000000, -1.000000000000000000 ) ) ;
#15037 = CARTESIAN_POINT ( 'NONE',  ( 9.734504863165533095, 30.79467112222051028, -9.359485933502590171 ) ) ;
#15038 = CARTESIAN_POINT ( 'NONE',  ( -2.048813550184076959, 56.60637244353360131, 13.34365525421965692 ) ) ;
#15039 = CARTESIAN_POINT ( 'NONE',  ( 11.37500000000039613, -8.290625000000000355, -4.711679271993002516 ) ) ;
#15040 = CARTESIAN_POINT ( 'NONE',  ( 13.29826067563849179, 33.34824635017109529, 2.325148998095313946 ) ) ;
#15041 = CARTESIAN_POINT ( 'NONE',  ( -3.737279461696752201E-15, 73.17999999999999261, -13.50000000000000000 ) ) ;
#15042 = CARTESIAN_POINT ( 'NONE',  ( 0.06721671892514809177, 40.17758380750846214, -13.49984309485949474 ) ) ;
#15043 = CARTESIAN_POINT ( 'NONE',  ( 11.76794919243112680, 23.58000000000001961, -3.823638476888993942 ) ) ;
#15044 = EDGE_CURVE ( 'NONE', #5339, #16171, #15304, .T. ) ;
#15045 = VERTEX_POINT ( 'NONE', #13724 ) ;
#15046 = CARTESIAN_POINT ( 'NONE',  ( -2.209542456836874003, 62.60055300686897795, 13.31796333730930471 ) ) ;
#15047 = ORIENTED_EDGE ( 'NONE', *, *, #2113, .F. ) ;
#15048 = CARTESIAN_POINT ( 'NONE',  ( -1.564113515457998370E-12, -53.03749999999988773, 18.62500000000000000 ) ) ;
#15049 = CARTESIAN_POINT ( 'NONE',  ( -13.50485324719562108, 43.92628281948966418, -0.1030264437535955285 ) ) ;
#15050 = CARTESIAN_POINT ( 'NONE',  ( 2.138189944381238661, 64.75688142232026223, 13.50000000000000000 ) ) ;
#15051 = CARTESIAN_POINT ( 'NONE',  ( -8.691771469529815392E-16, 35.67999999999998550, 14.19474002721660355 ) ) ;
#15052 = CARTESIAN_POINT ( 'NONE',  ( 18.62500000000064659, -10.44062499999995453, -7.714727599197336083 ) ) ;
#15053 = CARTESIAN_POINT ( 'NONE',  ( -10.10311990571781493, 67.58464977146856256, -8.954164421584090761 ) ) ;
#15054 = CARTESIAN_POINT ( 'NONE',  ( -18.62499999999935341, -66.63437499999983515, -7.714727599200458030 ) ) ;
#15055 = CARTESIAN_POINT ( 'NONE',  ( 13.14489197790636155, 54.32051714666025077, 3.086064228016605071 ) ) ;
#15056 = CARTESIAN_POINT ( 'NONE',  ( -0.6061693567267533167, 64.20179552098323938, -13.48666111876418583 ) ) ;
#15057 = EDGE_CURVE ( 'NONE', #15368, #16449, #3745, .T. ) ;
#15058 = ORIENTED_EDGE ( 'NONE', *, *, #3652, .F. ) ;
#15059 = CARTESIAN_POINT ( 'NONE',  ( 15.32135601632709410, 7.956016702382084915, -10.18318151426818297 ) ) ;
#15060 = CARTESIAN_POINT ( 'NONE',  ( -12.03451023656767127, 35.15595434393794250, 6.132305428729441843 ) ) ;
#15061 = EDGE_LOOP ( 'NONE', ( #9084, #7927, #2221, #11249 ) ) ;
#15062 = CARTESIAN_POINT ( 'NONE',  ( 13.05258666306970916, 78.55284067711124862, -3.446834127247557333 ) ) ;
#15063 = DIRECTION ( 'NONE',  ( 0.000000000000000000, 0.000000000000000000, -1.000000000000000000 ) ) ;
#15064 = CARTESIAN_POINT ( 'NONE',  ( 0.000000000000000000, 80.93000000000000682, 0.000000000000000000 ) ) ;
#15065 = CARTESIAN_POINT ( 'NONE',  ( 11.21626728703616571, 72.71231259042123440, -7.513034004964580070 ) ) ;
#15066 = CARTESIAN_POINT ( 'NONE',  ( 3.217771947876906680, 59.79570616790843474, 13.11091034625173712 ) ) ;
#15067 = CARTESIAN_POINT ( 'NONE',  ( 13.50000000000000000, 66.43000000000000682, 1.653273178848926867E-15 ) ) ;
#15068 = CARTESIAN_POINT ( 'NONE',  ( -12.79277096370526401, 52.77467266838400661, -4.312411596693917382 ) ) ;
#15069 = CARTESIAN_POINT ( 'NONE',  ( 3.636496289402157078, 41.02999999999999403, -11.19198476289190936 ) ) ;
#15070 = CARTESIAN_POINT ( 'NONE',  ( -9.520470885617715595, -17.36999999999999744, -6.917026985038136289 ) ) ;
#15071 = CARTESIAN_POINT ( 'NONE',  ( 13.49999999999999822, 59.27999999999998693, 4.386415899144237684 ) ) ;
#15072 = DIRECTION ( 'NONE',  ( 1.776356839400250465E-15, 0.000000000000000000, -1.000000000000000000 ) ) ;
#15073 = CARTESIAN_POINT ( 'NONE',  ( 4.801038565581039919, 68.85297145803022545, 12.61827525106671821 ) ) ;
#15074 = CARTESIAN_POINT ( 'NONE',  ( -2.819206891948295546, 37.28136828592626983, -13.20235427941665485 ) ) ;
#15075 = CARTESIAN_POINT ( 'NONE',  ( 3.708203932499368527, 4.696025403784437557, 11.41267819554184371 ) ) ;
#15076 = CARTESIAN_POINT ( 'NONE',  ( -13.16986379960055409, -50.95624999999989768, 13.16986379959834252 ) ) ;
#15077 = CARTESIAN_POINT ( 'NONE',  ( -9.939332794820023409, 74.28402178779931830, 9.138064150772017058 ) ) ;
#15078 = CARTESIAN_POINT ( 'NONE',  ( -9.395212350200784712, 76.54841060185640345, -9.694346819223181200 ) ) ;
#15079 = EDGE_CURVE ( 'NONE', #13170, #17257, #16645, .T. ) ;
#15080 = CARTESIAN_POINT ( 'NONE',  ( 7.312260103668256263E-16, 8.062177826491094379, -18.00000000000000000 ) ) ;
#15081 = CARTESIAN_POINT ( 'NONE',  ( 1.653273178848926472E-15, 80.93000000000000682, 13.50000000000000000 ) ) ;
#15082 = FILL_AREA_STYLE_COLOUR ( '', #1845 ) ;
#15083 = CARTESIAN_POINT ( 'NONE',  ( -11.76794919243112325, -5.220000000000004192, -3.823638476888998827 ) ) ;
#15084 = CARTESIAN_POINT ( 'NONE',  ( -9.520470885617715595, 47.62999999999999545, -6.917026985038136289 ) ) ;
#15085 = CARTESIAN_POINT ( 'NONE',  ( -4.171729424061787483, 1.329999999999997851, -12.83926296998457417 ) ) ;
#15086 = CARTESIAN_POINT ( 'NONE',  ( -2.235446294924008370, 32.59959283518442419, 13.31508909693261344 ) ) ;
#15087 = CARTESIAN_POINT ( 'NONE',  ( 13.19457708748799618, 75.53145179741177628, -2.867282558126743375 ) ) ;
#15088 = CARTESIAN_POINT ( 'NONE',  ( 15.12110384299646881, 2.066541229842317853E-14, -10.24447576295584383 ) ) ;
#15089 = SHAPE_REPRESENTATION_RELATIONSHIP ( 'NONE' , 'NONE' ,  #10992, #9886 ) ;
#15090 = CARTESIAN_POINT ( 'NONE',  ( -9.355789771963381796, 41.31352449815521766, 9.732436554501715520 ) ) ;
#15091 = CARTESIAN_POINT ( 'NONE',  ( 5.707630944344394663, 51.97262754088920644, -12.24211879259819469 ) ) ;
#15092 = CARTESIAN_POINT ( 'NONE',  ( -7.404093397872471449, 38.40322494662342478, 11.28901117625147599 ) ) ;
#15093 = CARTESIAN_POINT ( 'NONE',  ( 12.50000000000000000, 98.93000000000002103, 9.000000000000000000 ) ) ;
#15094 = CARTESIAN_POINT ( 'NONE',  ( 8.343458848123583849, 71.87999999999998124, -11.48378591275253768 ) ) ;
#15095 = CARTESIAN_POINT ( 'NONE',  ( 3.780205736804012180E-08, 55.17999999864077409, -13.50000000000000000 ) ) ;
#15096 = CARTESIAN_POINT ( 'NONE',  ( -12.03753084031560583, 49.70467287274419022, -6.112121115600539056 ) ) ;
#15097 = CARTESIAN_POINT ( 'NONE',  ( 9.423185512043215084, 63.04955960285478511, 9.674719739589008327 ) ) ;
#15098 = CARTESIAN_POINT ( 'NONE',  ( 12.36513741947113765, 42.23211346040410774, 5.417882651531068738 ) ) ;
#15099 = CARTESIAN_POINT ( 'NONE',  ( -18.00011380242310821, 8.062143945083761309, 0.1786886709309575549 ) ) ;
#15100 = CARTESIAN_POINT ( 'NONE',  ( 11.76794919243112325, 26.28000000000000824, 3.823638476888996163 ) ) ;
#15101 = EDGE_LOOP ( 'NONE', ( #9348, #3804, #3763, #10063 ) ) ;
#15102 = CARTESIAN_POINT ( 'NONE',  ( -7.272992578804310604, 72.38000000000000966, 10.01041549318726886 ) ) ;
#15103 = FACE_OUTER_BOUND ( 'NONE', #110, .T. ) ;
#15104 = CARTESIAN_POINT ( 'NONE',  ( -8.043339635996302306, -56.19374999999985931, -8.043339635997654113 ) ) ;
#15105 = CARTESIAN_POINT ( 'NONE',  ( 8.343458848123583849, 6.880000000000006999, -11.48378591275253768 ) ) ;
#15106 = EDGE_LOOP ( 'NONE', ( #5731, #11937, #10299, #12487, #10579, #15737 ) ) ;
#15107 = CARTESIAN_POINT ( 'NONE',  ( -5.291839448614410912, 43.37146548570319737, -12.42001919633759321 ) ) ;
#15108 = LINE ( 'NONE', #10990, #15277 ) ;
#15109 = CARTESIAN_POINT ( 'NONE',  ( 10.93522283957610775, 60.72922764856446776, -7.921801309275269709 ) ) ;
#15110 = AXIS2_PLACEMENT_3D ( 'NONE', #2209, #1072, #15730 ) ;
#15111 = CARTESIAN_POINT ( 'NONE',  ( 8.343458848123583849, 4.879999999999997229, -11.48378591275253768 ) ) ;
#15112 = CARTESIAN_POINT ( 'NONE',  ( -7.416407864998737942, 7.246025403784442709, 10.20780970022447853 ) ) ;
#15113 = CARTESIAN_POINT ( 'NONE',  ( 11.57317910393498828, 66.68907146314168699, -6.950662690379005859 ) ) ;
#15114 = CARTESIAN_POINT ( 'NONE',  ( 4.954131915168964895, 56.85870117836017812, 12.55812868081141076 ) ) ;
#15115 = CARTESIAN_POINT ( 'NONE',  ( 11.76794919243112325, 55.27999999999998693, 3.823638476888996607 ) ) ;
#15116 = CARTESIAN_POINT ( 'NONE',  ( -11.76794919243112325, 63.07999999999999119, 3.823638476888994386 ) ) ;
#15117 = CARTESIAN_POINT ( 'NONE',  ( -12.71445672950702210, 46.76596698851027156, -4.541269490033386091 ) ) ;
#15118 = EDGE_CURVE ( 'NONE', #4526, #16216, #4588, .T. ) ;
#15119 = CARTESIAN_POINT ( 'NONE',  ( 12.06082462307849923, 45.65376011911352805, -6.079388249483466566 ) ) ;
#15120 = FACE_OUTER_BOUND ( 'NONE', #7472, .T. ) ;
#15121 = DIRECTION ( 'NONE',  ( 1.000000000000000000, 0.000000000000000000, 0.000000000000000000 ) ) ;
#15122 = CARTESIAN_POINT ( 'NONE',  ( 0.3579478956273707824, 31.16713074970619601, -13.49560965235342280 ) ) ;
#15123 = CARTESIAN_POINT ( 'NONE',  ( -6.544256458472538895, 9.999999999999996447, -10.94569060336277211 ) ) ;
#15124 = CARTESIAN_POINT ( 'NONE',  ( 8.043339635997654113, -85.33124999999978400, -8.043339635996304082 ) ) ;
#15125 = CIRCLE ( 'NONE', #13721, 12.00000000000000178 ) ;
#15126 = CARTESIAN_POINT ( 'NONE',  ( -13.49999999999999822, 40.07999999999999829, 4.386415899144235020 ) ) ;
#15127 = CARTESIAN_POINT ( 'NONE',  ( 4.109698719430495473, 32.82776958409561985, 12.85927299696574977 ) ) ;
#15128 = CARTESIAN_POINT ( 'NONE',  ( -6.205905254110084535, 10.00000000000000000, 10.91717878730325353 ) ) ;
#15129 = CARTESIAN_POINT ( 'NONE',  ( 4.601630155619385043, 40.01437466971148638, -12.69233364863190339 ) ) ;
#15130 = CARTESIAN_POINT ( 'NONE',  ( -3.636496289402156190, 22.52999999999999403, 11.19198476289190758 ) ) ;
#15131 = EDGE_LOOP ( 'NONE', ( #13026, #16268 ) ) ;
#15132 = CARTESIAN_POINT ( 'NONE',  ( -3.934136427065950681, 62.53854296712907512, 12.91404697952921232 ) ) ;
#15133 = ORIENTED_EDGE ( 'NONE', *, *, #15310, .T. ) ;
#15134 = CARTESIAN_POINT ( 'NONE',  ( -7.409984580736203970E-16, -16.32000000000000028, 12.37355403259654985 ) ) ;
#15135 = CARTESIAN_POINT ( 'NONE',  ( 18.62500000000000000, -73.84999999999983800, 1.560692158462880521E-12 ) ) ;
#15136 = CARTESIAN_POINT ( 'NONE',  ( -13.25690904173389484, 43.83876739692001223, -2.587063218252659613 ) ) ;
#15137 = DIRECTION ( 'NONE',  ( 0.8660254037844348218, 0.000000000000000000, 0.5000000000000067724 ) ) ;
#15138 = CARTESIAN_POINT ( 'NONE',  ( 9.235077742801747647, 30.03187307936175543, 10.25657778616701599 ) ) ;
#15139 = CARTESIAN_POINT ( 'NONE',  ( 13.49999999999999822, 47.28000000000000114, 4.386415899144237684 ) ) ;
#15140 =( BOUNDED_CURVE ( )  B_SPLINE_CURVE ( 2, ( #1095, #11628, #15663, #11542, #11891, #4822, #13037, #14429, #17091, #2146, #8985, #4998, #6510 ),
 .UNSPECIFIED., .F., .F. ) 
 B_SPLINE_CURVE_WITH_KNOTS ( ( 3, 2, 2, 2, 2, 2, 3 ),
 ( 0.7916666666666666297, 0.7944444444444443976, 0.8000000000000000444, 0.8055555555555555802, 0.8111111111111111160, 0.8166666666666666519, 0.8194444444444444198 ),
 .UNSPECIFIED. ) 
 CURVE ( )  GEOMETRIC_REPRESENTATION_ITEM ( )  RATIONAL_B_SPLINE_CURVE ( ( 0.9755282581475768211, 0.9755282581475768211, 1.000000000000000000, 0.9510565162951535312, 1.000000000000000000, 0.9510565162951535312, 1.000000000000000000, 0.9510565162951535312, 1.000000000000000000, 0.9510565162951535312, 1.000000000000000000, 0.9755282581475768211, 0.9755282581475768211 ) ) 
 REPRESENTATION_ITEM ( '' )  );
#15141 = CARTESIAN_POINT ( 'NONE',  ( -8.931054703680040063, 46.52501327082484295, -10.16359813786777622 ) ) ;
#15142 = CARTESIAN_POINT ( 'NONE',  ( -4.753464114467623958, 67.35100568867868276, -12.64302991685488564 ) ) ;
#15143 = CARTESIAN_POINT ( 'NONE',  ( -7.714727599200466912, -54.14687499999985931, 18.62499999999935341 ) ) ;
#15144 = CARTESIAN_POINT ( 'NONE',  ( -1.003760800223034469E-07, 53.67999720368429450, 13.49999999999999822 ) ) ;
#15145 = CARTESIAN_POINT ( 'NONE',  ( -10.21286249403196855, 64.59057106318286401, -8.829037698084668762 ) ) ;
#15146 = ORIENTED_EDGE ( 'NONE', *, *, #933, .F. ) ;
#15147 = CARTESIAN_POINT ( 'NONE',  ( 15.78346433836034990, 8.055324230341707192, -8.708180880075682140 ) ) ;
#15148 = CARTESIAN_POINT ( 'NONE',  ( -11.52078070856594039, 34.66713973480176492, -7.043119858845972914 ) ) ;
#15149 = CARTESIAN_POINT ( 'NONE',  ( 8.043339635996300530, -64.51874999999984084, 8.043339635997654113 ) ) ;
#15150 = PRODUCT_RELATED_PRODUCT_CATEGORY ( 'part', '', ( #12276 ) ) ;
#15151 = VERTEX_POINT ( 'NONE', #7553 ) ;
#15152 = CARTESIAN_POINT ( 'NONE',  ( 13.39124523941554656, 78.37032605518025719, 1.711065265865323592 ) ) ;
#15153 = CARTESIAN_POINT ( 'NONE',  ( 10.92172942406178926, 47.12999999999999545, 7.935100905948387684 ) ) ;
#15154 = CARTESIAN_POINT ( 'NONE',  ( 7.500000000000000888, -25.65063367634387959, 7.726132535793202472 ) ) ;
#15155 = CARTESIAN_POINT ( 'NONE',  ( 4.670586549414562860, 73.01184521546099404, -12.66632117632807741 ) ) ;
#15156 = CARTESIAN_POINT ( 'NONE',  ( 3.500170436279223196, 79.05413282030319522, -13.04570395975783725 ) ) ;
#15157 = CARTESIAN_POINT ( 'NONE',  ( -8.549982208541774191E-16, -17.32000000000000384, 14.19474002721660355 ) ) ;
#15158 = CARTESIAN_POINT ( 'NONE',  ( -8.343458848123582072, 65.37999999999999545, 11.48378591275254124 ) ) ;
#15159 = CARTESIAN_POINT ( 'NONE',  ( -13.48061558364907064, 52.90503315535101336, -0.7233178539605096269 ) ) ;
#15160 = CARTESIAN_POINT ( 'NONE',  ( -7.576616670048093940E-16, 42.67999999999999972, 12.37355403259654985 ) ) ;
#15161 = CARTESIAN_POINT ( 'NONE',  ( -11.76794919243112325, -17.22000000000000597, -3.823638476888998827 ) ) ;
#15162 = CARTESIAN_POINT ( 'NONE',  ( 8.343458848123583849, 56.88000000000000256, -11.48378591275253768 ) ) ;
#15163 = EDGE_CURVE ( 'NONE', #15607, #743, #816, .T. ) ;
#15164 = DIRECTION ( 'NONE',  ( -6.302562568933760152E-16, -1.000000000000000000, 0.000000000000000000 ) ) ;
#15165 = CARTESIAN_POINT ( 'NONE',  ( -7.409984580736203970E-16, -1.320000000000003615, 12.37355403259654985 ) ) ;
#15166 = CARTESIAN_POINT ( 'NONE',  ( 11.48609513044766395, 69.16493330855622901, 7.097038714263399939 ) ) ;
#15167 = CARTESIAN_POINT ( 'NONE',  ( -8.891200544363830713E-16, 4.546025403784440755, 12.00000000000000000 ) ) ;
#15168 = CARTESIAN_POINT ( 'NONE',  ( 18.62499999999935341, -72.80937499999984652, 7.714727599200469577 ) ) ;
#15169 = CARTESIAN_POINT ( 'NONE',  ( -12.67808328063180845, 73.76223803303696513, -4.638750535666444463 ) ) ;
#15170 = CARTESIAN_POINT ( 'NONE',  ( -3.084225208773089477, 76.29063485233812969, -13.15363842553807494 ) ) ;
#15171 = DIRECTION ( 'NONE',  ( -0.000000000000000000, 1.000000000000000000, -0.000000000000000000 ) ) ;
#15172 = CARTESIAN_POINT ( 'NONE',  ( -15.58845726811976995, 7.773118517290098062, -11.00000000000018119 ) ) ;
#15173 = CARTESIAN_POINT ( 'NONE',  ( 4.171729424061789260, 3.830000000000000071, 12.83926296998457239 ) ) ;
#15174 = CARTESIAN_POINT ( 'NONE',  ( -13.49999999999999822, 32.78000000000001535, -4.386415899144240349 ) ) ;
#15175 = CARTESIAN_POINT ( 'NONE',  ( -9.520470885617715595, -11.36999999999999744, -6.917026985038136289 ) ) ;
#15176 = CARTESIAN_POINT ( 'NONE',  ( 2.272985001014427393E-15, 38.17999999999999972, -12.37355403259654807 ) ) ;
#15177 = CARTESIAN_POINT ( 'NONE',  ( -13.49999999999999822, -16.22000000000000597, -4.386415899144240349 ) ) ;
#15178 = CARTESIAN_POINT ( 'NONE',  ( -3.265813649003837860, 32.56277205055386759, 13.10951091463926055 ) ) ;
#15179 = CARTESIAN_POINT ( 'NONE',  ( 13.48416359079525151, 75.45253600662924498, -0.6538687915017138419 ) ) ;
#15180 = CARTESIAN_POINT ( 'NONE',  ( 10.51254708004915983, -1.361280322109189478E-15, -4.824314191992851164 ) ) ;
#15181 = AXIS2_PLACEMENT_3D ( 'NONE', #12230, #12140, #5350 ) ;
#15182 = CARTESIAN_POINT ( 'NONE',  ( 7.272992578804311492, 34.87999999999999545, -10.01041549318726709 ) ) ;
#15183 = CARTESIAN_POINT ( 'NONE',  ( 13.50000000000000000, 80.43000000000000682, 1.653273178848926867E-15 ) ) ;
#15184 = CARTESIAN_POINT ( 'NONE',  ( 9.428830175397949986, 51.81010302066297868, -9.668537834129738329 ) ) ;
#15185 = CARTESIAN_POINT ( 'NONE',  ( -1.554078682580832815, 38.62412002689448798, 13.41025849265453473 ) ) ;
#15186 = CARTESIAN_POINT ( 'NONE',  ( 5.409153947552197472, 36.98379089016496835, -12.36981397998242649 ) ) ;
#15187 = CARTESIAN_POINT ( 'NONE',  ( -9.708203932499390731, 0.7639745962155688463, -7.053423027509696297 ) ) ;
#15188 = CYLINDRICAL_SURFACE ( 'NONE', #11485, 1.999999999999998224 ) ;
#15189 = CARTESIAN_POINT ( 'NONE',  ( 7.102532611500677717, 62.94396966511739322, 11.48060114064993975 ) ) ;
#15190 = CARTESIAN_POINT ( 'NONE',  ( 13.32040245924266664, 42.35294902285478003, 2.194828684655724338 ) ) ;
#15191 = CARTESIAN_POINT ( 'NONE',  ( 1.538839542171267061, 38.73533021766907325, 13.41224767058500333 ) ) ;
#15192 = CIRCLE ( 'NONE', #4775, 26.00000000000000355 ) ;
#15193 = CARTESIAN_POINT ( 'NONE',  ( -7.272992578804307939, 21.48000000000001108, -10.01041549318726886 ) ) ;
#15194 = ORIENTED_EDGE ( 'NONE', *, *, #5631, .T. ) ;
#15195 = CARTESIAN_POINT ( 'NONE',  ( -9.520470885617717371, 69.23000000000000398, 6.917026985038133624 ) ) ;
#15196 = CARTESIAN_POINT ( 'NONE',  ( -12.00000000000000178, 3.646025403784438623, -3.899036354794879422 ) ) ;
#15197 = CARTESIAN_POINT ( 'NONE',  ( 11.37500000000039435, -50.99062499999988063, -4.711679271993003404 ) ) ;
#15198 = CARTESIAN_POINT ( 'NONE',  ( 13.50000000000000000, 6.430000000000005045, 1.734723475976807094E-15 ) ) ;
#15199 = EDGE_LOOP ( 'NONE', ( #16213, #6229, #7909, #2305 ) ) ;
#15200 = CARTESIAN_POINT ( 'NONE',  ( -2.220955663942571601, 43.25985729847043615, -13.31607982724954908 ) ) ;
#15201 = CARTESIAN_POINT ( 'NONE',  ( -5.441113646577473872, 0.000000000000000000, -25.42428528562855305 ) ) ;
#15202 = CARTESIAN_POINT ( 'NONE',  ( -10.92172942406179104, 0.2300000000000079758, 7.935100905948385908 ) ) ;
#15203 = CARTESIAN_POINT ( 'NONE',  ( 25.42428528562852819, 0.000000000000000000, 5.441113646577569796 ) ) ;
#15204 = DIRECTION ( 'NONE',  ( -0.000000000000000000, -1.000000000000000000, -0.000000000000000000 ) ) ;
#15205 = CARTESIAN_POINT ( 'NONE',  ( 12.94155673114020466, 66.29238691916880555, 3.842733075138333287 ) ) ;
#15206 = CARTESIAN_POINT ( 'NONE',  ( 11.15568599528430838, 57.14407707936145187, 7.606331343502261255 ) ) ;
#15207 = CARTESIAN_POINT ( 'NONE',  ( 9.520470885617717371, 58.73000000000000398, -6.917026985038131848 ) ) ;
#15208 = CARTESIAN_POINT ( 'NONE',  ( 10.92172942406179104, 32.72999999999999687, -7.935100905948385908 ) ) ;
#15209 = CARTESIAN_POINT ( 'NONE',  ( 11.76794919243112680, 67.57999999999998408, -3.823638476888993942 ) ) ;
#15210 = EDGE_CURVE ( 'NONE', #1419, #15151, #7765, .T. ) ;
#15211 = CARTESIAN_POINT ( 'NONE',  ( -11.71715498535849598, 46.68080331322232013, -6.708422292409551346 ) ) ;
#15212 = AXIS2_PLACEMENT_3D ( 'NONE', #4761, #5686, #8336 ) ;
#15213 = CARTESIAN_POINT ( 'NONE',  ( 5.636143214428637194, 45.97535775804710312, -12.26722223200532902 ) ) ;
#15214 = CARTESIAN_POINT ( 'NONE',  ( 7.416407864998774357, 8.113974596215598467, 10.20780970022453182 ) ) ;
#15215 = CARTESIAN_POINT ( 'NONE',  ( 0.6924984764758361777, 8.027888383433445796, 18.11551784069756721 ) ) ;
#15216 = CARTESIAN_POINT ( 'NONE',  ( 7.607743402570670277, 30.89476037788184470, -11.17066045873822233 ) ) ;
#15217 = CARTESIAN_POINT ( 'NONE',  ( -7.461870820705466478, 56.40082279287123157, 11.26181808124483830 ) ) ;
#15218 = CARTESIAN_POINT ( 'NONE',  ( -2.090093454172745613, 50.60485299099218537, 13.33722994085978719 ) ) ;
#15219 = CARTESIAN_POINT ( 'NONE',  ( 11.71562641685611794, 33.17875202474539265, 6.766063318502479440 ) ) ;
#15220 = CARTESIAN_POINT ( 'NONE',  ( -9.033826763038382168, 9.999999999999998224, 8.302007722878922635 ) ) ;
#15221 = CARTESIAN_POINT ( 'NONE',  ( -9.479632845647650186, 8.043285765338840321, -15.38489371673200878 ) ) ;
#15222 = ORIENTED_EDGE ( 'NONE', *, *, #11296, .F. ) ;
#15223 = CARTESIAN_POINT ( 'NONE',  ( -11.04935343432774708, 62.22247568111082217, 7.756490358654122730 ) ) ;
#15224 = ORIENTED_EDGE ( 'NONE', *, *, #8576, .T. ) ;
#15225 = CARTESIAN_POINT ( 'NONE',  ( -13.40968305279137951, 40.98484619147922814, 1.574467244674663036 ) ) ;
#15226 = CARTESIAN_POINT ( 'NONE',  ( -3.636496289402152637, -14.66999999999999638, -11.19198476289190936 ) ) ;
#15227 = CARTESIAN_POINT ( 'NONE',  ( -7.714727599200466912, -18.69687499999997726, 18.62499999999935341 ) ) ;
#15228 = CARTESIAN_POINT ( 'NONE',  ( -12.72580279456753338, 43.76730851413559265, -4.505998233414108434 ) ) ;
#15229 = CARTESIAN_POINT ( 'NONE',  ( 2.138189944381242213, 66.10311857767973720, -13.49999999999999822 ) ) ;
#15230 = CARTESIAN_POINT ( 'NONE',  ( 13.50000000000000355, 33.57999999999999829, -4.386415899144233244 ) ) ;
#15231 = CARTESIAN_POINT ( 'NONE',  ( -4.171729424061791036, 43.53000000000000114, 12.83926296998457239 ) ) ;
#15232 = CIRCLE ( 'NONE', #7087, 3.624999999999999556 ) ;
#15233 = CARTESIAN_POINT ( 'NONE',  ( -2.934267639516605630, 46.28547539380033982, -13.18180308497758446 ) ) ;
#15234 = CARTESIAN_POINT ( 'NONE',  ( -11.72621171495925196, 67.68154214080810505, -6.689257902045856241 ) ) ;
#15235 = CARTESIAN_POINT ( 'NONE',  ( -13.16986379959834252, -82.24374999999977831, -13.16986379960055409 ) ) ;
#15236 = CARTESIAN_POINT ( 'NONE',  ( 6.499702057654023868, 53.91894888444889489, 11.83264119668203485 ) ) ;
#15237 = EDGE_LOOP ( 'NONE', ( #14596, #14264 ) ) ;
#15238 = CARTESIAN_POINT ( 'NONE',  ( -10.31288091114224059, 64.59587999935689595, -8.711744710682491899 ) ) ;
#15239 = ORIENTED_EDGE ( 'NONE', *, *, #4247, .T. ) ;
#15240 = CARTESIAN_POINT ( 'NONE',  ( -5.247208035731191877, 34.36974467868986949, -12.43902619372017782 ) ) ;
#15241 = CARTESIAN_POINT ( 'NONE',  ( 9.538709233711902776E-13, -54.11249999999986926, -11.37500000000000000 ) ) ;
#15242 = CARTESIAN_POINT ( 'NONE',  ( 11.52123726438447626, 78.16718586782270961, 7.042369149511602977 ) ) ;
#15243 = CARTESIAN_POINT ( 'NONE',  ( -15.78346433836042095, 8.055324230341707192, 8.708180880075572006 ) ) ;
#15244 = CARTESIAN_POINT ( 'NONE',  ( 7.500000000000001776, -27.45244706754152020, -4.067225351102822017 ) ) ;
#15245 = CARTESIAN_POINT ( 'NONE',  ( 11.69054898252628050, 72.17893444877771003, 6.754223243015324840 ) ) ;
#15246 = CARTESIAN_POINT ( 'NONE',  ( -7.272992578804310604, 28.38000000000000966, 10.01041549318726709 ) ) ;
#15247 = CARTESIAN_POINT ( 'NONE',  ( -10.92172942406178926, 64.62999999999999545, -7.935100905948389460 ) ) ;
#15248 = CARTESIAN_POINT ( 'NONE',  ( -4.420108738712346330, 52.33898909862991644, -12.75633360914648229 ) ) ;
#15249 = CARTESIAN_POINT ( 'NONE',  ( 7.272992578804311492, 40.87999999999998835, -10.01041549318726709 ) ) ;
#15250 = CARTESIAN_POINT ( 'NONE',  ( -4.171729424061791036, 61.53000000000000114, 12.83926296998457239 ) ) ;
#15251 = CARTESIAN_POINT ( 'NONE',  ( 0.000000000000000000, 9.000000000000000000, 0.000000000000000000 ) ) ;
#15252 = CARTESIAN_POINT ( 'NONE',  ( 11.76794919243112680, -0.4200000000000027045, -3.823638476888993942 ) ) ;
#15253 = CARTESIAN_POINT ( 'NONE',  ( 10.31646666059287476, 69.09600980556707839, 8.710257868796588809 ) ) ;
#15254 = CARTESIAN_POINT ( 'NONE',  ( -2.835384746425102964, 37.28194995933510114, -13.19889313174409473 ) ) ;
#15255 = CARTESIAN_POINT ( 'NONE',  ( -13.49999999999999822, 73.08000000000001251, 4.386415899144235020 ) ) ;
#15256 = CARTESIAN_POINT ( 'NONE',  ( -18.62500000000064659, -99.86562499999978115, 7.714727599197333419 ) ) ;
#15257 = CARTESIAN_POINT ( 'NONE',  ( -11.38516945207351405, 73.65842273094972370, -7.254522738815065708 ) ) ;
#15258 = CARTESIAN_POINT ( 'NONE',  ( -1.101621291205112207, 76.21958249968859889, -13.46178648949251588 ) ) ;
#15259 = CARTESIAN_POINT ( 'NONE',  ( -3.641410069088633961, 79.31075509186923966, -13.00494094948426316 ) ) ;
#15260 = CARTESIAN_POINT ( 'NONE',  ( -3.708203932499367195, 0.1960254037844345598, -11.41267819554184548 ) ) ;
#15261 = CARTESIAN_POINT ( 'NONE',  ( 8.486513546626678561, 8.030919929218461206, -16.00650186718814894 ) ) ;
#15262 = CARTESIAN_POINT ( 'NONE',  ( 2.621994543952811015E-15, 29.18000000000000327, -14.19474002721660355 ) ) ;
#15263 = CARTESIAN_POINT ( 'NONE',  ( 3.636496289402154414, -4.169999999999999929, 11.19198476289190758 ) ) ;
#15264 = EDGE_CURVE ( 'NONE', #8372, #17275, #17006, .T. ) ;
#15265 = CARTESIAN_POINT ( 'NONE',  ( 9.520470885617717371, 40.72999999999999687, -6.917026985038131848 ) ) ;
#15266 = UNCERTAINTY_MEASURE_WITH_UNIT (LENGTH_MEASURE( 1.000000000000000082E-05 ), #8539, 'distance_accuracy_value', 'NONE');
#15267 = CARTESIAN_POINT ( 'NONE',  ( 10.92172942406178926, -17.86999999999999744, 7.935100905948385908 ) ) ;
#15268 = CARTESIAN_POINT ( 'NONE',  ( 7.999999999999885425, 7.170708369609772426, 19.79695994079632726 ) ) ;
#15269 = CARTESIAN_POINT ( 'NONE',  ( 1.312945976112900981, 74.72720796987070457, 13.43600633030649227 ) ) ;
#15270 = CARTESIAN_POINT ( 'NONE',  ( 4.246271870433876217, 5.783373742538367096E-16, -15.51202266832556198 ) ) ;
#15271 = CARTESIAN_POINT ( 'NONE',  ( -13.50000000000000000, 84.93000000000000682, -3.306546357697853733E-15 ) ) ;
#15272 = CARTESIAN_POINT ( 'NONE',  ( -2.264479525414730077, 58.26142199067226812, -13.30896360304205039 ) ) ;
#15273 = CARTESIAN_POINT ( 'NONE',  ( -1.388205926214359787, 38.63012733182188185, 13.42855087378624468 ) ) ;
#15274 = DIRECTION ( 'NONE',  ( -0.000000000000000000, 1.000000000000000000, -0.000000000000000000 ) ) ;
#15275 = CARTESIAN_POINT ( 'NONE',  ( -10.92172942406178926, 69.62999999999999545, -7.935100905948389460 ) ) ;
#15276 = CARTESIAN_POINT ( 'NONE',  ( -4.382329622040107786, 49.33761423158443904, -12.76923448255947413 ) ) ;
#15277 = VECTOR ( 'NONE', #112, 1000.000000000000000 ) ;
#15278 = CARTESIAN_POINT ( 'NONE',  ( 2.650574835413161523, 62.77529302382879450, 13.23723914315057293 ) ) ;
#15279 = CARTESIAN_POINT ( 'NONE',  ( 5.499638061715979909, 41.87941307834116600, 12.32899955262698732 ) ) ;
#15280 = CARTESIAN_POINT ( 'NONE',  ( 8.525489938592672345, 48.85322366431354624, -10.46738712784432934 ) ) ;
#15281 = CARTESIAN_POINT ( 'NONE',  ( -3.636496289402156190, 25.52999999999999758, 11.19198476289190758 ) ) ;
#15282 = ORIENTED_EDGE ( 'NONE', *, *, #640, .T. ) ;
#15283 = CARTESIAN_POINT ( 'NONE',  ( -9.520470885617717371, 66.23000000000000398, 6.917026985038133624 ) ) ;
#15284 = CARTESIAN_POINT ( 'NONE',  ( 4.711679271994911211, 4.128125000000008704, -11.37499999999960743 ) ) ;
#15285 = CARTESIAN_POINT ( 'NONE',  ( 11.37499999999960210, -82.20937499999980957, 4.711679271994917428 ) ) ;
#15286 = ORIENTED_EDGE ( 'NONE', *, *, #8898, .T. ) ;
#15287 = ADVANCED_FACE ( 'NONE', ( #3644 ), #12676, .F. ) ;
#15288 = CARTESIAN_POINT ( 'NONE',  ( 2.924053257345435538E-06, 68.68008145904181561, 13.49999999999936584 ) ) ;
#15289 = CARTESIAN_POINT ( 'NONE',  ( 0.000000000000000000, 80.93000000000000682, 0.000000000000000000 ) ) ;
#15290 = CARTESIAN_POINT ( 'NONE',  ( -4.171729424061787483, 2.329999999999998739, -12.83926296998457417 ) ) ;
#15291 = CARTESIAN_POINT ( 'NONE',  ( 18.62499999999934985, -15.60937499999996270, 7.714727599200467800 ) ) ;
#15292 = CARTESIAN_POINT ( 'NONE',  ( 11.83941929220342537, 66.18971953923538365, 6.486927149400845138 ) ) ;
#15293 = CARTESIAN_POINT ( 'NONE',  ( 10.71075049650908895, 57.11789055711182073, 8.217759637934333838 ) ) ;
#15294 = CARTESIAN_POINT ( 'NONE',  ( 2.272985001014427788E-15, 59.17999999999998550, -12.37355403259654985 ) ) ;
#15295 = CARTESIAN_POINT ( 'NONE',  ( -7.272992578804310604, 66.37999999999999545, 10.01041549318726709 ) ) ;
#15296 = AXIS2_PLACEMENT_3D ( 'NONE', #16185, #5619, #2841 ) ;
#15297 = CARTESIAN_POINT ( 'NONE',  ( -11.61613876028604331, 46.67376607488575502, -6.881206147996638656 ) ) ;
#15298 = CARTESIAN_POINT ( 'NONE',  ( 7.426031545778958964, 45.90225655064444510, -11.27414640185626205 ) ) ;
#15299 = DIRECTION ( 'NONE',  ( -0.000000000000000000, 1.000000000000000000, -0.000000000000000000 ) ) ;
#15300 = CARTESIAN_POINT ( 'NONE',  ( 11.28170547357727749, 30.70818519455021800, -7.414394825668972011 ) ) ;
#15301 = CARTESIAN_POINT ( 'NONE',  ( -12.72210886894176696, 56.09309001809862849, 4.516451198278201851 ) ) ;
#15302 = CARTESIAN_POINT ( 'NONE',  ( 2.138189944381238661, 52.75688142232026934, 13.50000000000000000 ) ) ;
#15303 = CARTESIAN_POINT ( 'NONE',  ( 13.28530447619198185, 33.34560229784237606, 2.398270177113091428 ) ) ;
#15304 = LINE ( 'NONE', #16559, #8851 ) ;
#15305 = CARTESIAN_POINT ( 'NONE',  ( 10.32321619528713086, 39.76356552170057057, -8.699496154864482023 ) ) ;
#15306 = ORIENTED_EDGE ( 'NONE', *, *, #6794, .T. ) ;
#15307 = CARTESIAN_POINT ( 'NONE',  ( -12.49324912787944264, 62.11632128283577714, 5.121990780005423183 ) ) ;
#15308 = EDGE_LOOP ( 'NONE', ( #6061, #16290, #14347, #16174 ) ) ;
#15309 = VECTOR ( 'NONE', #17135, 1000.000000000000000 ) ;
#15310 = EDGE_CURVE ( 'NONE', #13044, #4352, #34, .T. ) ;
#15311 = CARTESIAN_POINT ( 'NONE',  ( 2.621994543952811015E-15, 28.18000000000000682, -14.19474002721660355 ) ) ;
#15312 = CARTESIAN_POINT ( 'NONE',  ( 18.62500000000064659, -24.94062499999996518, -7.714727599197336083 ) ) ;
#15313 = CARTESIAN_POINT ( 'NONE',  ( 11.69049970947668982, 48.17901677739538968, 6.751497366717108761 ) ) ;
#15314 = DIRECTION ( 'NONE',  ( -8.862145109134287319E-17, 1.000000000000000000, 0.000000000000000000 ) ) ;
#15315 = CARTESIAN_POINT ( 'NONE',  ( -13.49999999999999822, 31.77999999999999758, -4.386415899144240349 ) ) ;
#15316 = CARTESIAN_POINT ( 'NONE',  ( -0.1281060804169691925, 46.18460550068364512, -13.49947775182521248 ) ) ;
#15317 = CARTESIAN_POINT ( 'NONE',  ( -7.462108197810392696, 67.45929967586793907, -11.25098269314221078 ) ) ;
#15318 = CARTESIAN_POINT ( 'NONE',  ( -18.62500000000064659, -68.71562499999981810, 7.714727599197333419 ) ) ;
#15319 = CARTESIAN_POINT ( 'NONE',  ( 5.999104543695027658, 53.89865356422039611, 12.09973455174266022 ) ) ;
#15320 =( REPRESENTATION_RELATIONSHIP ('NONE','NONE', #7275, #10992 ) REPRESENTATION_RELATIONSHIP_WITH_TRANSFORMATION ( #12010 )SHAPE_REPRESENTATION_RELATIONSHIP( ) );
#15321 = ORIENTED_EDGE ( 'NONE', *, *, #1110, .F. ) ;
#15322 = CARTESIAN_POINT ( 'NONE',  ( -11.76794919243112325, 80.92999999999767624, -5.919446256302011733E-11 ) ) ;
#15323 = ORIENTED_EDGE ( 'NONE', *, *, #15617, .T. ) ;
#15324 = CARTESIAN_POINT ( 'NONE',  ( -22.50000000000000355, -14.00000000000000533, -2.204364238465235822E-15 ) ) ;
#15325 = CARTESIAN_POINT ( 'NONE',  ( -8.165485012641067186, 34.49031512341151284, -10.75073694722957640 ) ) ;
#15326 = CARTESIAN_POINT ( 'NONE',  ( -4.711679271994916540, -28.09687499999992966, 11.37499999999960210 ) ) ;
#15327 = DIRECTION ( 'NONE',  ( 0.000000000000000000, -1.000000000000000000, 0.000000000000000000 ) ) ;
#15328 = CARTESIAN_POINT ( 'NONE',  ( 0.000000000000000000, -22.00000000000000000, 0.000000000000000000 ) ) ;
#15329 = CARTESIAN_POINT ( 'NONE',  ( 7.999999999999904965, 0.000000000000000000, 17.32050807568881368 ) ) ;
#15330 = CARTESIAN_POINT ( 'NONE',  ( -8.343458848123578520, 36.47999999999998977, -11.48378591275254124 ) ) ;
#15331 = B_SPLINE_CURVE_WITH_KNOTS ( 'NONE', 3,
 ( #8538, #14067, #4715, #13888, #560, #11348, #14151, #10288, #1787, #11520, #15385, #473, #10037, #1952, #8708, #12925, #16897, #5882, #4801, #16640, #809, #12754, #3292, #5967, #7377, #3201, #643, #8621, #13975, #6054, #1870, #8794, #12668, #12845, #16723, #4630, #11436, #15471, #10203, #3382, #2040, #15555, #7464, #733, #6141, #3467, #15993, #7895, #5242, #13097, #17068, #983, #11951, #12271, #3637, #5154, #3816, #5066, #7635, #17155, #9315, #6897, #10955, #6396, #2464, #13013, #13272, #17331, #168, #17244, #10461, #10628, #5572, #15821, #3897, #1160, #7721, #14665, #3550, #11779, #6570, #2292, #3726, #2554, #7983, #13186, #2378, #2208, #9144, #9229, #8964, #14491, #14320, #13352, #4972, #7813, #10547, #1481, #893, #6306, #11691, #1071, #6484, #10375, #14404, #11869, #15729, #15907, #9051, #14583, #9641, #15342, #16415, #7070, #14022, #1912, #5747, #14991, #2883, #7239, #7330, #8315, #13670, #9906, #8578, #6986, #15166, #16591, #3064, #11043, #11131, #1744, #3242, #5834, #4499, #4317, #8491, #15253, #9727, #13755, #4586, #600, #12713, #12361, #8403, #6012, #1655, #12625, #9819, #16323, #13929, #3152, #513, #1823, #5921, #1567, #13842, #16504, #12454, #4409, #8665, #256, #338, #11302, #4229, #15073, #428, #16679, #7156, #5662, #12541, #9994, #11217, #2972, #12802, #6100, #14110, #13057, #11649, #851, #939, #774, #7678, #7771, #12885, #6350, #9004, #15513, #5017, #13142 ),
 .UNSPECIFIED., .F., .F.,
 ( 4, 2, 2, 1, 2, 2, 2, 1, 1, 2, 2, 1, 1, 2, 2, 2, 2, 2, 2, 1, 1, 1, 2, 2, 2, 2, 2, 1, 2, 2, 2, 2, 2, 2, 2, 2, 2, 2, 1, 1, 2, 2, 2, 2, 2, 2, 1, 1, 1, 1, 2, 2, 2, 1, 2, 2, 1, 1, 1, 2, 2, 2, 2, 2, 2, 1, 1, 2, 2, 2, 2, 2, 2, 1, 1, 2, 1, 1, 2, 2, 1, 2, 2, 2, 2, 1, 1, 1, 2, 2, 2, 2, 2, 2, 2, 2, 2, 1, 1, 1, 1, 2, 2, 1, 1, 2, 2, 2, 2, 1, 1, 1, 2, 4 ),
 ( 0.2108027933308743440, 0.2109176789523807827, 0.2110325645738872213, 0.2112623358169000987, 0.2117218783029258811, 0.2126409632749773904, 0.2144791332190804645, 0.2147089044620933418, 0.2148237900835997805, 0.2148381507862880957, 0.2148453311376322394, 0.2148525114889763832, 0.2148812328943529859, 0.2149386757051061358, 0.2153982181911315019, 0.2163173031631822063, 0.2167768456492075724, 0.2167912063518958599, 0.2168055670545841751, 0.2168342884599607501, 0.2168917312707139278, 0.2170066168922202832, 0.2172363881352329940, 0.2181554731072838094, 0.2186150155933092309, 0.2187299012148155863, 0.2187586226201921891, 0.2187873440255687640, 0.2188447868363219695, 0.2190745580793347080, 0.2195341005653601574, 0.2197638718083728959, 0.2198213146191260736, 0.2198787574298792791, 0.2199936430513856345, 0.2209127280234366164, 0.2209701708341897941, 0.2209845315368781093, 0.2209988922395663968, 0.2210276136449429996, 0.2211424992664493550, 0.2213722705094621213, 0.2218318129954875984, 0.2227508979675386080, 0.2232104404535640851, 0.2232248011562523726, 0.2232391618589406879, 0.2232678832643172906, 0.2233253260750704683, 0.2234402116965768514, 0.2236699829395895900, 0.2255081528836916094, 0.2264272378557426468, 0.2265421234772490022, 0.2265564841799373175, 0.2265636645312814612, 0.2265708448826256050, 0.2265995662880022077, 0.2266570090987553576, 0.2268867803417680684, 0.2273463228277934345, 0.2282654077998441944, 0.2284951790428568774, 0.2285095397455451649, 0.2285239004482334524, 0.2285526218536100551, 0.2286100646643632051, 0.2287249502858695605, 0.2291844927718948988, 0.2301035777439456309, 0.2303333489869583139, 0.2304482346084646416, 0.2304769560138412166, 0.2305056774192178193, 0.2305631202299709970, 0.2310226627159963908, 0.2312524339590090738, 0.2313673195805154292, 0.2314247623912686069, 0.2314534837966451819, 0.2314822052020217846, 0.2319417476880472062, 0.2324012901740726278, 0.2324156508767609153, 0.2324300115794492028, 0.2324587329848258055, 0.2325161757955789832, 0.2326310614170853386, 0.2328608326600980771, 0.2337799176321490036, 0.2342394601181744529, 0.2344692313611871637, 0.2346990026041999022, 0.2356180875762508009, 0.2365371725483016996, 0.2365946153590548773, 0.2366520581698080550, 0.2367669437913144104, 0.2369967150343271212, 0.2374562575203525705, 0.2376860287633652813, 0.2377147501687418563, 0.2377291108714301437, 0.2377434715741184590, 0.2378009143848716089, 0.2379158000063779643, 0.2383753424924033304, 0.2388348849784287242, 0.2388636063838052992, 0.2388923277891819019, 0.2389497705999350519, 0.2390646562214414073, 0.2392944274644540903, 0.2402135124365048502 ),
 .UNSPECIFIED. ) ;
#15332 = CARTESIAN_POINT ( 'NONE',  ( 12.47883071023084334, 72.24232604971501814, 5.156649975335684921 ) ) ;
#15333 = CARTESIAN_POINT ( 'NONE',  ( 11.76794919243112325, 29.28000000000001180, 3.823638476888996163 ) ) ;
#15334 = CARTESIAN_POINT ( 'NONE',  ( -4.171729424061791036, 62.53000000000000114, 12.83926296998457239 ) ) ;
#15335 = CARTESIAN_POINT ( 'NONE',  ( -5.830206929847885355, 52.39226344610381858, -12.17615902335279543 ) ) ;
#15336 = CARTESIAN_POINT ( 'NONE',  ( -9.520470885617715595, 41.63000000000000256, -6.917026985038136289 ) ) ;
#15337 = CARTESIAN_POINT ( 'NONE',  ( -11.76794919243112325, -13.91999999999999815, 3.823638476888994386 ) ) ;
#15338 = CARTESIAN_POINT ( 'NONE',  ( 2.607531440858944223E-15, 57.17999999999999261, -14.19474002721660355 ) ) ;
#15339 = CARTESIAN_POINT ( 'NONE',  ( 1.528574478876175036, 50.73496190250285309, 13.41318330975730966 ) ) ;
#15340 = EDGE_CURVE ( 'NONE', #10383, #14262, #13335, .T. ) ;
#15341 = CARTESIAN_POINT ( 'NONE',  ( 3.636496289402157078, 0.03000000000000224709, -11.19198476289190936 ) ) ;
#15342 = CARTESIAN_POINT ( 'NONE',  ( 12.78125498241015734, 69.27338024102353131, 4.346469460005440766 ) ) ;
#15343 = CARTESIAN_POINT ( 'NONE',  ( -1.337701960717650129, 37.22806044761306055, -13.43546765959366596 ) ) ;
#15344 = CARTESIAN_POINT ( 'NONE',  ( -18.62500000000064659, -83.21562499999981810, 7.714727599197333419 ) ) ;
#15345 = CARTESIAN_POINT ( 'NONE',  ( -10.66802778328771595, 73.61539763354224419, -8.273749749751072358 ) ) ;
#15346 = DIRECTION ( 'NONE',  ( 0.000000000000000000, 1.000000000000000000, 0.000000000000000000 ) ) ;
#15347 = CARTESIAN_POINT ( 'NONE',  ( 9.708203932499371192, 8.596025403784453900, -7.053423027509677645 ) ) ;
#15348 = CARTESIAN_POINT ( 'NONE',  ( 9.869431986045617222, 8.002175404975853112, -15.32050807568866624 ) ) ;
#15349 = CARTESIAN_POINT ( 'NONE',  ( -7.272992578804310604, -7.620000000000000995, 10.01041549318726709 ) ) ;
#15350 = CARTESIAN_POINT ( 'NONE',  ( 7.272992578804311492, 37.87999999999999545, -10.01041549318726886 ) ) ;
#15351 =( BOUNDED_CURVE ( )  B_SPLINE_CURVE ( 2, ( #15021, #14522, #14698, #8431, #13785, #7843, #6518, #13216, #1103, #17364, #17274, #2585, #16110, #8017, #10578, #5360, #4348, #369, #10746, #4020, #3846, #5278, #5774, #9757, #3932, #1599, #5188, #9349, #13384, #7928, #12483, #13301, #12393, #1274, #15854, #8343, #2913, #3762, #14614, #11983, #9174, #2409, #7015, #10662, #15939, #9262, #6686, #2497, #1192, #3001, #6603, #16026, #12068, #17445, #283, #13699, #9434, #15102, #5692, #11072, #16445, #1683, #7099, #8692, #11423, #11245, #10021, #9848, #5951, #16795, #2107, #11331, #798, #6128, #7182, #3184, #629, #8782, #15195, #4441, #3095, #16709, #13958, #7451, #4527, #11507, #1855, #7269, #16534, #12570, #12652, #5866, #16883, #457, #14138, #6040, #542, #8521, #15283, #16624, #8606, #1773, #13871, #9934, #4614, #15369, #3275, #4701, #14052, #1939, #10106, #4789, #12741, #10190, #7362, #15457, #3368, #11159, #15543, #2026, #12831, #718, #3455, #8870, #14223, #7534, #12914, #11680, #13339, #11767, #2369, #11594, #4873, #7802, #15627, #3535, #6208, #9218, #13086, #16971, #8950, #9131, #2195, #10276, #10450, #2542, #6294, #13173, #14308, #17143, #7623, #15718, #5052, #15983, #15809, #13000, #882, #11938, #17056, #4961, #10364, #3622, #9039, #15897, #7708, #14392, #6471, #2281, #971, #6384, #1059, #3713, #14480, #11857, #17232, #5142, #10534, #14569, #3805, #2453, #7883, #13260, #1147, #6558, #17319, #7970, #5231, #10616, #3886, #9303, #14654, #10785, #6816, #11054, #86, #12023, #17402, #6997, #8059, #1230, #13423, #16151, #5317, #10966, #2716, #6727, #1493, #2627, #1312, #3975, #2894, #5491, #5586, #12373, #14822, #8145, #12105, #10872, #9738, #10701, #8237, #266, #15084, #4059, #16334, #4242, #16069, #16426, #2983, #5674, #1579, #4150, #179, #9475, #8326, #12193, #4330, #14738, #17486, #6908, #13508, #9651, #9387, #5401, #1400, #2805, #13681, #16242, #9562, #14912, #13597, #12284, #8414, #15001, #6642, #11312, #8503, #12724, #8676, #7251, #611, #12635, #6108, #11490, #5756, #4422, #11140, #16515, #15265, #9831, #524, #14033, #5932, #13852, #3162, #16689, #698, #3252, #1921, #1755, #4597, #3433, #2005, #1834, #16776, #15176, #10003, #15350, #5846, #10174, #11229, #10088, #7341, #13765, #6020, #8763, #3076, #16603, #11404, #4684, #12465, #12552, #16864, #8589, #4510, #15439, #7166, #14118, #9916, #13940, #1667, #438, #3348, #7431, #12811, #4769, #15523, #7081, #349, #7514, #12978, #1124, #782, #16950, #6189, #11575, #10339, #4851, #7687, #9107, #13064, #3516, #15694, #11743, #13237 ),
 .UNSPECIFIED., .F., .F. ) 
 B_SPLINE_CURVE_WITH_KNOTS ( ( 3, 2, 2, 2, 2, 2, 2, 2, 2, 2, 2, 2, 2, 2, 2, 2, 2, 2, 2, 2, 2, 2, 2, 2, 2, 2, 2, 2, 2, 2, 2, 2, 2, 2, 2, 2, 2, 2, 2, 2, 2, 2, 2, 2, 2, 2, 2, 2, 2, 2, 2, 2, 2, 2, 2, 2, 2, 2, 2, 2, 2, 2, 2, 2, 2, 2, 2, 2, 2, 2, 2, 2, 2, 2, 2, 2, 2, 2, 2, 2, 2, 2, 2, 2, 2, 2, 2, 2, 2, 2, 2, 2, 2, 2, 2, 2, 2, 2, 2, 2, 2, 2, 2, 2, 2, 2, 2, 2, 2, 2, 2, 2, 2, 2, 2, 2, 2, 2, 2, 2, 2, 2, 2, 2, 2, 2, 2, 2, 2, 2, 2, 2, 2, 2, 2, 2, 2, 2, 2, 2, 2, 2, 2, 2, 2, 2, 2, 2, 2, 2, 2, 2, 2, 2, 2, 2, 2, 2, 2, 2, 2, 2, 2, 2, 2, 2, 2, 3 ),
 ( 0.05660416580082960891, 0.06226458238090768621, 0.06792499896098576351, 0.07358541554106384774, 0.07924583212114191810, 0.08490624870121998846, 0.09056666528129808658, 0.09622708186137615693, 0.1018874984414542412, 0.1075479150215323254, 0.1132083316016103819, 0.1188687481816884661, 0.1245291647617665504, 0.1301895813418446068, 0.1358499979219227050, 0.1415104145020008031, 0.1471708310820788457, 0.1528312476621569438, 0.1584916642422350419, 0.1641520808223131123, 0.1698124974023911549, 0.1754729139824692530, 0.1811333305625473233, 0.1867937471426253937, 0.1924541637227034918, 0.1981145803027815622, 0.2037749968828596603, 0.2094354134629377029, 0.2150958300430157732, 0.2207562466230938714, 0.2264166632031719417, 0.2320770797832500398, 0.2377374963633281102, 0.2433979129434062083, 0.2490583295234842509, 0.2547187461035623213, 0.2603791626836404194, 0.2660395792637185175, 0.2716999958437965601, 0.2773604124238746582, 0.2830208290039527563, 0.2886812455840307989, 0.2943416621641088415, 0.3000020787441869952, 0.3056624953242650378, 0.3113229119043431359, 0.3169833284844211785, 0.3226437450644992211, 0.3283041616445774302, 0.3339645782246554728, 0.3396249948047335154, 0.3452854113848115580, 0.3509458279648896561, 0.3566062445449676988, 0.3622666611250458524, 0.3679270777051239505, 0.3735874942852019376, 0.3792479108652800357, 0.3849083274453581338, 0.3905687440254362874, 0.3962291606055143300, 0.4018895771855923726, 0.4075499937656704708, 0.4132104103457484578, 0.4188708269258265560, 0.4245312435059047651, 0.4301916600859828077, 0.4358520766660608503, 0.4415124932461388929, 0.4471729098262169910, 0.4528333264062949781, 0.4584937429863731873, 0.4641541595664512854, 0.4698145761465292725, 0.4754749927266073706, 0.4811354093066854132, 0.4867958258867636223, 0.4924562424668416094, 0.4981166590469197075, 0.5037770756269978056, 0.5094374922070757927, 0.5150979087871538908, 0.5207583253672318779, 0.5264187419473100871, 0.5320791585273881852, 0.5377395751074662833, 0.5433999916875442704, 0.5490604082676222575, 0.5547208248477004666, 0.5603812414277785647, 0.5660416580078566628, 0.5717020745879347610, 0.5773624911680127481, 0.5830229077480908462, 0.5886833243281688333, 0.5943437409082470424, 0.6000041574883251405, 0.6056645740684031276, 0.6113249906484811147, 0.6169854072285593238, 0.6226458238086374219, 0.6283062403887155201, 0.6339666569687935072, 0.6396270735488716053, 0.6452874901289497034, 0.6509479067090276905, 0.6566083232891058996, 0.6622687398691839977, 0.6679291564492619848, 0.6735895730293400829, 0.6792499896094181810, 0.6849104061894962792, 0.6905708227695742663, 0.6962312393496524754, 0.7018916559297304625, 0.7075520725098084496, 0.7132124890898866587, 0.7188729056699647568, 0.7245333222500428549, 0.7301937388301208420, 0.7358541554101989401, 0.7415145719902770383, 0.7471749885703550254, 0.7528354051504332345, 0.7584958217305113326, 0.7641562383105893197, 0.7698166548906673068, 0.7754770714707455159, 0.7811374880508236140, 0.7867979046309016011, 0.7924583212109798103, 0.7981187377910577974, 0.8037791543711357845, 0.8094395709512138826, 0.8150999875312920917, 0.8207604041113701898, 0.8264208206914481769, 0.8320812372715262750, 0.8377416538516043731, 0.8434020704316823602, 0.8490624870117604583, 0.8547229035918386675, 0.8603833201719166546, 0.8660437367519946417, 0.8717041533320728508, 0.8773645699121509489, 0.8830249864922289360, 0.8886854030723070341, 0.8943458196523851322, 0.9000062362324631193, 0.9056666528125412174, 0.9113270693926194266, 0.9169874859726975247, 0.9226479025527755118, 0.9283083191328536099, 0.9339687357129317080, 0.9396291522930098061, 0.9452895688730877932, 0.9509499854531660024, 0.9566104020332439895, 0.9622708186133219765, 0.9679312351934001857, 0.9735916517734782838, 0.9792520683535562709, 0.9849124849336343690, 0.9905729015137124671, 0.9962333180937904542, 1.000000000000000000 ),
 .UNSPECIFIED. ) 
 CURVE ( )  GEOMETRIC_REPRESENTATION_ITEM ( )  RATIONAL_B_SPLINE_CURVE ( ( 0.9999999999996016520, 0.9510565162955518792, 1.000000000000000000, 0.9510565162951535312, 1.000000000000000000, 0.9510565162951535312, 1.000000000000000000, 0.9510565162951535312, 1.000000000000000000, 0.9510565162951535312, 1.000000000000000000, 0.9510565162951535312, 1.000000000000000000, 0.9510565162951535312, 1.000000000000000000, 0.9510565162951535312, 1.000000000000000000, 0.9510565162951535312, 1.000000000000000000, 0.9510565162951535312, 1.000000000000000000, 0.9510565162951535312, 1.000000000000000000, 0.9510565162951535312, 1.000000000000000000, 0.9510565162951535312, 1.000000000000000000, 0.9510565162951535312, 1.000000000000000000, 0.9510565162951535312, 1.000000000000000000, 0.9510565162951535312, 1.000000000000000000, 0.9510565162951535312, 1.000000000000000000, 0.9510565162951535312, 1.000000000000000000, 0.9510565162951535312, 1.000000000000000000, 0.9510565162951535312, 1.000000000000000000, 0.9510565162951535312, 1.000000000000000000, 0.9510565162951535312, 1.000000000000000000, 0.9510565162951535312, 1.000000000000000000, 0.9510565162951535312, 1.000000000000000000, 0.9510565162951535312, 1.000000000000000000, 0.9510565162951535312, 1.000000000000000000, 0.9510565162951535312, 1.000000000000000000, 0.9510565162951535312, 1.000000000000000000, 0.9510565162951535312, 1.000000000000000000, 0.9510565162951535312, 1.000000000000000000, 0.9510565162951535312, 1.000000000000000000, 0.9510565162951535312, 1.000000000000000000, 0.9510565162951535312, 1.000000000000000000, 0.9510565162951535312, 1.000000000000000000, 0.9510565162951535312, 1.000000000000000000, 0.9510565162951535312, 1.000000000000000000, 0.9510565162951535312, 1.000000000000000000, 0.9510565162951535312, 1.000000000000000000, 0.9510565162951535312, 1.000000000000000000, 0.9510565162951535312, 1.000000000000000000, 0.9510565162951535312, 1.000000000000000000, 0.9510565162951535312, 1.000000000000000000, 0.9510565162951535312, 1.000000000000000000, 0.9510565162951535312, 1.000000000000000000, 0.9510565162951535312, 1.000000000000000000, 0.9510565162951535312, 1.000000000000000000, 0.9510565162951535312, 1.000000000000000000, 0.9510565162951535312, 1.000000000000000000, 0.9510565162951535312, 1.000000000000000000, 0.9510565162951535312, 1.000000000000000000, 0.9510565162951535312, 1.000000000000000000, 0.9510565162951535312, 1.000000000000000000, 0.9510565162951535312, 1.000000000000000000, 0.9510565162951535312, 1.000000000000000000, 0.9510565162951535312, 1.000000000000000000, 0.9510565162951535312, 1.000000000000000000, 0.9510565162951535312, 1.000000000000000000, 0.9510565162951535312, 1.000000000000000000, 0.9510565162951535312, 1.000000000000000000, 0.9510565162951535312, 1.000000000000000000, 0.9510565162951535312, 1.000000000000000000, 0.9510565162951535312, 1.000000000000000000, 0.9510565162951535312, 1.000000000000000000, 0.9510565162951535312, 1.000000000000000000, 0.9510565162951535312, 1.000000000000000000, 0.9510565162951535312, 1.000000000000000000, 0.9510565162951535312, 1.000000000000000000, 0.9510565162951535312, 1.000000000000000000, 0.9510565162951535312, 1.000000000000000000, 0.9510565162951535312, 1.000000000000000000, 0.9510565162951535312, 1.000000000000000000, 0.9510565162951535312, 1.000000000000000000, 0.9510565162951535312, 1.000000000000000000, 0.9510565162951535312, 1.000000000000000000, 0.9510565162951535312, 1.000000000000000000, 0.9510565162951535312, 1.000000000000000000, 0.9510565162951535312, 1.000000000000000000, 0.9510565162951535312, 1.000000000000000000, 0.9510565162951535312, 1.000000000000000000, 0.9510565162951535312, 1.000000000000000000, 0.9510565162951535312, 1.000000000000000000, 0.9510565162951535312, 1.000000000000000000, 0.9510565162951535312, 1.000000000000000000, 0.9510565162951535312, 1.000000000000000000, 0.9510565162951535312, 1.000000000000000000, 0.9510565162951535312, 1.000000000000000000, 0.9510565162951535312, 1.000000000000000000, 0.9510565162951535312, 1.000000000000000000, 0.9510565162951535312, 1.000000000000000000, 0.9510565162951535312, 1.000000000000000000, 0.9510565162951535312, 1.000000000000000000, 0.9510565162951535312, 1.000000000000000000, 0.9510565162951535312, 1.000000000000000000, 0.9510565162951535312, 1.000000000000000000, 0.9510565162951535312, 1.000000000000000000, 0.9510565162951535312, 1.000000000000000000, 0.9510565162951535312, 1.000000000000000000, 0.9510565162951535312, 1.000000000000000000, 0.9510565162951535312, 1.000000000000000000, 0.9510565162951535312, 1.000000000000000000, 0.9510565162951535312, 1.000000000000000000, 0.9510565162951535312, 1.000000000000000000, 0.9510565162951535312, 1.000000000000000000, 0.9510565162951535312, 1.000000000000000000, 0.9510565162951535312, 1.000000000000000000, 0.9510565162951535312, 1.000000000000000000, 0.9510565162951535312, 1.000000000000000000, 0.9510565162951535312, 1.000000000000000000, 0.9510565162951535312, 1.000000000000000000, 0.9510565162951535312, 1.000000000000000000, 0.9510565162951535312, 1.000000000000000000, 0.9510565162951535312, 1.000000000000000000, 0.9510565162951535312, 1.000000000000000000, 0.9510565162951535312, 1.000000000000000000, 0.9510565162951535312, 1.000000000000000000, 0.9510565162951535312, 1.000000000000000000, 0.9510565162951535312, 1.000000000000000000, 0.9510565162951535312, 1.000000000000000000, 0.9510565162951535312, 1.000000000000000000, 0.9510565162951535312, 1.000000000000000000, 0.9510565162951535312, 1.000000000000000000, 0.9510565162951535312, 1.000000000000000000, 0.9510565162951535312, 1.000000000000000000, 0.9510565162951535312, 1.000000000000000000, 0.9510565162951535312, 1.000000000000000000, 0.9510565162951535312, 1.000000000000000000, 0.9510565162951535312, 1.000000000000000000, 0.9510565162951535312, 1.000000000000000000, 0.9510565162951535312, 1.000000000000000000, 0.9510565162951535312, 1.000000000000000000, 0.9510565162951535312, 1.000000000000000000, 0.9510565162951535312, 1.000000000000000000, 0.9510565162951535312, 1.000000000000000000, 0.9510565162951535312, 1.000000000000000000, 0.9510565162951535312, 1.000000000000000000, 0.9510565162951535312, 1.000000000000000000, 0.9510565162951535312, 1.000000000000000000, 0.9510565162951535312, 1.000000000000000000, 0.9510565162951535312, 1.000000000000000000, 0.9510565162951535312, 1.000000000000000000, 0.9510565162951535312, 1.000000000000000000, 0.9510565162951535312, 1.000000000000000000, 0.9510565162951535312, 1.000000000000000000, 0.9510565162951535312, 1.000000000000000000, 0.9510565162951535312, 1.000000000000000000, 0.9510565162951535312, 1.000000000000000000, 0.9510565162951535312, 1.000000000000000000, 0.9510565162951535312, 1.000000000000000000, 0.9510565162951535312, 1.000000000000000000, 0.9510565162951535312, 1.000000000000000000, 0.9510565162951535312, 1.000000000000000000, 0.9510565162951535312, 1.000000000000000000, 0.9510565162951535312, 1.000000000000000000, 0.9510565162951535312, 1.000000000000000000, 0.9510565162951535312, 1.000000000000000000, 0.9510565162951535312, 1.000000000000000000, 0.9510565162951535312, 1.000000000000000000, 0.9510565162951535312, 1.000000000000000000, 0.9510565162951535312, 1.000000000000000000, 0.9510565162951535312, 1.000000000000000000, 0.9510565162951535312, 1.000000000000000000, 0.9510565162951535312, 1.000000000000000000, 0.9510565162951535312, 1.000000000000000000, 0.9510565162951535312, 1.000000000000000000, 0.9510565162951535312, 1.000000000000000000, 0.9510565162951535312, 1.000000000000000000, 0.9674309245812854341, 0.9782075447827165426 ) ) 
 REPRESENTATION_ITEM ( '' )  );
#15352 = CARTESIAN_POINT ( 'NONE',  ( 13.50000000000000355, -17.42000000000000526, -4.386415899144233244 ) ) ;
#15353 = CARTESIAN_POINT ( 'NONE',  ( 1.628308837847167748E-06, 32.68004529479373588, 13.49999999999980460 ) ) ;
#15354 = CARTESIAN_POINT ( 'NONE',  ( 9.949328106897166180, 75.07664185812758717, 9.126035338817397147 ) ) ;
#15355 = CARTESIAN_POINT ( 'NONE',  ( 13.49999999999999822, 3.280000000000003801, 4.386415899144236796 ) ) ;
#15356 =( NAMED_UNIT ( * ) PLANE_ANGLE_UNIT ( ) SI_UNIT ( $, .RADIAN. ) );
#15357 = CARTESIAN_POINT ( 'NONE',  ( 8.343458848123578520, 79.98000000000001819, 11.48378591275254124 ) ) ;
#15358 = CIRCLE ( 'NONE', #16491, 1.999999999999998224 ) ;
#15359 = CARTESIAN_POINT ( 'NONE',  ( 6.498476362382647586, 51.94114444125180086, -11.84129758499792118 ) ) ;
#15360 = DIRECTION ( 'NONE',  ( 0.000000000000000000, 0.000000000000000000, 1.000000000000000000 ) ) ;
#15361 = LINE ( 'NONE', #16615, #6407 ) ;
#15362 = CARTESIAN_POINT ( 'NONE',  ( -2.138189944381257757, 69.25688142232027644, -13.49999999999999289 ) ) ;
#15363 = CARTESIAN_POINT ( 'NONE',  ( -17.32050807568886697, 0.000000000000000000, 9.999999999999838352 ) ) ;
#15364 = CARTESIAN_POINT ( 'NONE',  ( 2.599693433324294922, 62.77350978289579331, 13.24734751974565405 ) ) ;
#15365 = CARTESIAN_POINT ( 'NONE',  ( 3.088734071207799303, 41.79106346645730241, 13.14190885100032524 ) ) ;
#15366 = CARTESIAN_POINT ( 'NONE',  ( 10.55941645560348441, 48.75061515200597029, -8.411729401910850612 ) ) ;
#15367 = CARTESIAN_POINT ( 'NONE',  ( -11.76794919243112325, 21.93000000000000682, -2.602085213965210642E-15 ) ) ;
#15368 = VERTEX_POINT ( 'NONE', #6148 ) ;
#15369 = CARTESIAN_POINT ( 'NONE',  ( 2.272985001014427393E-15, 65.18000000000000682, -12.37355403259654807 ) ) ;
#15370 = CARTESIAN_POINT ( 'NONE',  ( 9.538709233711902776E-13, -30.21249999999990976, -11.37500000000000178 ) ) ;
#15371 = CARTESIAN_POINT ( 'NONE',  ( 8.043339635997654113, -35.38124999999991616, -8.043339635996304082 ) ) ;
#15372 = CARTESIAN_POINT ( 'NONE',  ( 10.92172942406178926, 3.129999999999993676, 7.935100905948385908 ) ) ;
#15373 = CARTESIAN_POINT ( 'NONE',  ( -3.636496289402152637, 33.32999999999999829, -11.19198476289190936 ) ) ;
#15374 = CARTESIAN_POINT ( 'NONE',  ( -2.875760791593931984E-14, 76.17999999999999261, -13.50000000000000000 ) ) ;
#15375 = CARTESIAN_POINT ( 'NONE',  ( 13.49999999999999822, -1.720000000000005302, 4.386415899144237684 ) ) ;
#15376 = CARTESIAN_POINT ( 'NONE',  ( -18.62499999999935341, -40.58437499999990905, -7.714727599200458918 ) ) ;
#15377 = CARTESIAN_POINT ( 'NONE',  ( 10.32274762114379030, 66.09624816351212928, 8.700950685072003310 ) ) ;
#15378 = CARTESIAN_POINT ( 'NONE',  ( 4.171729424061791924, 79.03000000000000114, -12.83926296998457239 ) ) ;
#15379 = CIRCLE ( 'NONE', #8371, 2.000000000000001776 ) ;
#15380 = CARTESIAN_POINT ( 'NONE',  ( -9.520470885617717371, 54.23000000000000398, 6.917026985038133624 ) ) ;
#15381 = CARTESIAN_POINT ( 'NONE',  ( -10.99999999999979394, 0.000000000000000000, -15.58845726812003996 ) ) ;
#15382 = CARTESIAN_POINT ( 'NONE',  ( -11.76794919243112325, 56.77999999999998693, -3.823638476888998827 ) ) ;
#15383 = CARTESIAN_POINT ( 'NONE',  ( -13.31105111643021921, 46.85093201765869253, -2.250770146535703287 ) ) ;
#15384 = CARTESIAN_POINT ( 'NONE',  ( 10.70331455173479895, 45.74252489688407053, -8.227460180060322870 ) ) ;
#15385 = CARTESIAN_POINT ( 'NONE',  ( 3.493247654510983846, 70.05461554162307891, -13.06995608569233092 ) ) ;
#15386 = EDGE_CURVE ( 'NONE', #568, #11530, #11539, .T. ) ;
#15387 = CARTESIAN_POINT ( 'NONE',  ( 1.645451467107275745, 7.815250021811909420, 18.85000554241879200 ) ) ;
#15388 = CARTESIAN_POINT ( 'NONE',  ( 8.369696161555634006, 30.86039719007353455, -10.59237420471009195 ) ) ;
#15389 = CARTESIAN_POINT ( 'NONE',  ( -13.46224735791354732, 55.96492138559692364, 1.008931430782477268 ) ) ;
#15390 = CARTESIAN_POINT ( 'NONE',  ( 13.50000000000000355, 53.58000000000000540, -4.386415899144233244 ) ) ;
#15391 = CARTESIAN_POINT ( 'NONE',  ( 1.138962821616983367, 32.72095444842646828, 13.45206967035641377 ) ) ;
#15392 = CARTESIAN_POINT ( 'NONE',  ( 4.346632539395717032, 43.02368370212016657, -12.78113607336223367 ) ) ;
#15393 = CARTESIAN_POINT ( 'NONE',  ( 11.20568860838524294, 39.71295177364815032, -7.528793318710608418 ) ) ;
#15394 = ORIENTED_EDGE ( 'NONE', *, *, #4043, .T. ) ;
#15395 = CARTESIAN_POINT ( 'NONE',  ( -13.16850383217373732, 61.82452929595484648, -2.976946126390717318 ) ) ;
#15396=STYLED_ITEM('',(#17519),#3202);
#15397 = VERTEX_POINT ( 'NONE', #9930 ) ;
#15398 = CARTESIAN_POINT ( 'NONE',  ( -13.49999999999999822, 34.78000000000001535, -4.386415899144240349 ) ) ;
#15399 = CARTESIAN_POINT ( 'NONE',  ( 18.62499999999934630, -32.25937499999992042, 7.714727599200467800 ) ) ;
#15400 = CARTESIAN_POINT ( 'NONE',  ( 11.53697122679876408, 48.16844816899800463, 7.012046851884700338 ) ) ;
#15401 = DIRECTION ( 'NONE',  ( 0.000000000000000000, -1.000000000000000000, 0.000000000000000000 ) ) ;
#15402 = CARTESIAN_POINT ( 'NONE',  ( 8.343458848123578520, 35.97999999999999687, 11.48378591275254124 ) ) ;
#15403 = CARTESIAN_POINT ( 'NONE',  ( 4.171729424061789260, 37.82999999999999829, 12.83926296998457417 ) ) ;
#15404 = CARTESIAN_POINT ( 'NONE',  ( 9.746503595109638596, -1.242015572811693166E-15, 9.216735997558972215 ) ) ;
#15405 = AXIS2_PLACEMENT_3D ( 'NONE', #7289, #11181, #8626 ) ;
#15406 = ADVANCED_FACE ( 'NONE', ( #2103 ), #12910, .T. ) ;
#15407 = CARTESIAN_POINT ( 'NONE',  ( -1.315351892621634544, 46.22726836446648946, -13.43749779991192561 ) ) ;
#15408 = DIRECTION ( 'NONE',  ( 0.000000000000000000, -1.000000000000000000, 0.000000000000000000 ) ) ;
#15409 = CARTESIAN_POINT ( 'NONE',  ( 8.043339635996302306, -40.61874999999988489, 8.043339635997654113 ) ) ;
#15410 = CARTESIAN_POINT ( 'NONE',  ( 9.212593542616069442, 54.03942132565033063, 9.869137508411661486 ) ) ;
#15411 = VERTEX_POINT ( 'NONE', #4869 ) ;
#15412 = CARTESIAN_POINT ( 'NONE',  ( -1.403062250848142511, 64.23045450618263885, -13.42962668392956616 ) ) ;
#15413 = ORIENTED_EDGE ( 'NONE', *, *, #13992, .T. ) ;
#15414 = CARTESIAN_POINT ( 'NONE',  ( -2.838270712586780596E-14, 67.18000000000000682, -13.50000000000000178 ) ) ;
#15415 = CARTESIAN_POINT ( 'NONE',  ( -4.329644013675561176, 34.33569415333381158, -12.78730092188580691 ) ) ;
#15416 = CARTESIAN_POINT ( 'NONE',  ( -8.043339635996300530, -13.49374999999998614, -8.043339635997652337 ) ) ;
#15417 = CARTESIAN_POINT ( 'NONE',  ( 8.248096366247494871, 77.99385762200095940, 10.69720316962921913 ) ) ;
#15418 = CARTESIAN_POINT ( 'NONE',  ( 8.343458848123580296, 46.97999999999999687, 11.48378591275253768 ) ) ;
#15419 = VECTOR ( 'NONE', #5006, 1000.000000000000000 ) ;
#15420 = CARTESIAN_POINT ( 'NONE',  ( 0.000000000000000000, 30.93000000000001393, -13.50000000000000000 ) ) ;
#15421 = CARTESIAN_POINT ( 'NONE',  ( 7.500000000000001776, -24.46203974633109368, -8.709571264514700317 ) ) ;
#15422 = CARTESIAN_POINT ( 'NONE',  ( 10.67593876640750317, 72.11592638041871339, 8.262829459856675385 ) ) ;
#15423 = CARTESIAN_POINT ( 'NONE',  ( -9.520470885617715595, 27.63000000000001677, -6.917026985038136289 ) ) ;
#15424 = CARTESIAN_POINT ( 'NONE',  ( 13.50000000000000355, 66.57999999999999829, -4.386415899144233244 ) ) ;
#15425 = CARTESIAN_POINT ( 'NONE',  ( -2.380357500337397791, 52.26558885175427349, -13.28850035324038359 ) ) ;
#15426 = CARTESIAN_POINT ( 'NONE',  ( 2.272985001014427788E-15, 38.17999999999999972, -12.37355403259654985 ) ) ;
#15427 = CARTESIAN_POINT ( 'NONE',  ( 8.343458848123578520, 52.97999999999999687, 11.48378591275254124 ) ) ;
#15428 = CARTESIAN_POINT ( 'NONE',  ( 0.000000000000000000, 0.000000000000000000, 0.000000000000000000 ) ) ;
#15429 = CARTESIAN_POINT ( 'NONE',  ( 3.636496289402154414, -1.170000000000004370, 11.19198476289190758 ) ) ;
#15430 = CARTESIAN_POINT ( 'NONE',  ( -2.911921858601246527, 68.57532333875593622, 13.18921981885233130 ) ) ;
#15431 = CARTESIAN_POINT ( 'NONE',  ( 1.561832610794586538E-12, -37.46249999999991331, -18.62500000000000000 ) ) ;
#15432 = CARTESIAN_POINT ( 'NONE',  ( -1.732050807569007977, 7.773118517290099838, 18.99999999999998224 ) ) ;
#15433 = CARTESIAN_POINT ( 'NONE',  ( 7.714727599200458030, -3.121874999999992628, -18.62499999999934985 ) ) ;
#15434 = CARTESIAN_POINT ( 'NONE',  ( -11.69088730954973876, 73.67895630682167507, -6.753829726051608695 ) ) ;
#15435 = DIRECTION ( 'NONE',  ( -1.000000000000000000, -1.445602896647338917E-16, 0.000000000000000000 ) ) ;
#15436 = DIRECTION ( 'NONE',  ( -1.000000000000000000, -1.734723475976807094E-16, -0.000000000000000000 ) ) ;
#15437 = CARTESIAN_POINT ( 'NONE',  ( 8.258382090122001529, 7.982365321444606643, -16.32862261014056671 ) ) ;
#15438 = CARTESIAN_POINT ( 'NONE',  ( 8.343458848123578520, 27.98000000000000753, 11.48378591275254124 ) ) ;
#15439 = CARTESIAN_POINT ( 'NONE',  ( 2.272985001014427393E-15, 35.17999999999999261, -12.37355403259654807 ) ) ;
#15440 = CARTESIAN_POINT ( 'NONE',  ( -7.999999999999670486, 5.918584287042171432, -24.73863375370606477 ) ) ;
#15441 = CARTESIAN_POINT ( 'NONE',  ( -1.812614935732535848, 32.61479078993660607, 13.37801144487990612 ) ) ;
#15442 = CARTESIAN_POINT ( 'NONE',  ( -2.811464633627016061E-07, 74.67999216907730897, 13.49999999999999289 ) ) ;
#15443 = EDGE_CURVE ( 'NONE', #5905, #12574, #8602, .T. ) ;
#15444 = CARTESIAN_POINT ( 'NONE',  ( 1.469576158976824144E-15, 9.000000000000000000, 12.00000000000000178 ) ) ;
#15445 = CARTESIAN_POINT ( 'NONE',  ( 10.92172942406179104, 80.72999999999998977, -7.935100905948385908 ) ) ;
#15446 = CARTESIAN_POINT ( 'NONE',  ( 11.82310823617331330, 51.67149392221477910, -6.517150710059238961 ) ) ;
#15447 = CARTESIAN_POINT ( 'NONE',  ( -1.704182853630322292, 38.61868516537028029, 13.39237762325557135 ) ) ;
#15448 = CARTESIAN_POINT ( 'NONE',  ( 8.416301635034747264, 36.85828208203987799, -10.55640874431936993 ) ) ;
#15449 = CARTESIAN_POINT ( 'NONE',  ( 11.37500000000039435, -67.64062499999984368, -4.711679271993004292 ) ) ;
#15450 = CARTESIAN_POINT ( 'NONE',  ( 0.000000000000000000, 9.000000000000000000, 0.000000000000000000 ) ) ;
#15451 = DIRECTION ( 'NONE',  ( -0.000000000000000000, 1.000000000000000000, -0.000000000000000000 ) ) ;
#15452 = CARTESIAN_POINT ( 'NONE',  ( 0.3122628659426803788, 62.69122775878508946, 13.49642344175948061 ) ) ;
#15453 = CARTESIAN_POINT ( 'NONE',  ( 5.571623316695888839, 41.88219105858915725, 12.29678795757967080 ) ) ;
#15454 = CARTESIAN_POINT ( 'NONE',  ( 13.22950857473560049, 48.52495454413182330, -2.688921183273661697 ) ) ;
#15455 = CARTESIAN_POINT ( 'NONE',  ( -7.272992578804307939, 18.48000000000000398, -10.01041549318726886 ) ) ;
#15456 = EDGE_LOOP ( 'NONE', ( #15693, #881, #2566, #5164 ) ) ;
#15457 = CARTESIAN_POINT ( 'NONE',  ( -7.576616670048093940E-16, 63.67999999999998550, 12.37355403259654807 ) ) ;
#15458 = CARTESIAN_POINT ( 'NONE',  ( 13.16986379959833897, -73.91874999999977547, 13.16986379960055409 ) ) ;
#15459 = CARTESIAN_POINT ( 'NONE',  ( 9.538709233711902776E-13, -70.76249999999983231, -11.37500000000000000 ) ) ;
#15460 = CARTESIAN_POINT ( 'NONE',  ( -4.171729424061791036, -0.4699999999999981970, 12.83926296998457239 ) ) ;
#15461 = CARTESIAN_POINT ( 'NONE',  ( 11.76794919243112325, 32.28000000000000114, 3.823638476888996163 ) ) ;
#15462 = CARTESIAN_POINT ( 'NONE',  ( -11.29885598845502059, 80.92999999999994998, -4.264693269864170411 ) ) ;
#15463 = EDGE_CURVE ( 'NONE', #5515, #3211, #8162, .T. ) ;
#15464 = CARTESIAN_POINT ( 'NONE',  ( 13.16986379960055054, -35.38124999999991616, -13.16986379959834430 ) ) ;
#15465 = CARTESIAN_POINT ( 'NONE',  ( 12.93521420879763362, 66.29158821686850445, 3.864030656794251950 ) ) ;
#15466 = LINE ( 'NONE', #8701, #2815 ) ;
#15467 = CARTESIAN_POINT ( 'NONE',  ( -3.636496289402155746, 48.52999999999999403, 11.19198476289190936 ) ) ;
#15468 = CARTESIAN_POINT ( 'NONE',  ( 4.171729424061791924, 33.02999999999999403, -12.83926296998457239 ) ) ;
#15469 = CARTESIAN_POINT ( 'NONE',  ( -13.31132898414792542, 47.01062904578743940, 2.286098758061895886 ) ) ;
#15470 = CARTESIAN_POINT ( 'NONE',  ( 11.74912485249524607, 45.67681818464819088, -6.649168124183248985 ) ) ;
#15471 = CARTESIAN_POINT ( 'NONE',  ( 9.075450842952271557, 69.82754448784227463, -10.00762726697219129 ) ) ;
#15472 = CARTESIAN_POINT ( 'NONE',  ( -9.708203932499369415, 7.363974596215575374, 7.053423027509678533 ) ) ;
#15473 = CARTESIAN_POINT ( 'NONE',  ( 11.91445496772408141, 30.66470696577163579, -6.348179239168573851 ) ) ;
#15474 = CARTESIAN_POINT ( 'NONE',  ( -13.13757147891543653, 56.04209669737164035, 3.157802568303226032 ) ) ;
#15475 = DIRECTION ( 'NONE',  ( -0.000000000000000000, -1.000000000000000000, -0.000000000000000000 ) ) ;
#15476 = CARTESIAN_POINT ( 'NONE',  ( 9.229767010897823809, 33.04026619113517427, 9.852102493543972273 ) ) ;
#15477 = CARTESIAN_POINT ( 'NONE',  ( 3.966527692860394971, 43.03741821288255665, -12.90466901633432606 ) ) ;
#15478 = CARTESIAN_POINT ( 'NONE',  ( 10.32978028215595856, 39.76320980175390929, -8.691700943171158045 ) ) ;
#15479 = ORIENTED_EDGE ( 'NONE', *, *, #1972, .T. ) ;
#15480 = CARTESIAN_POINT ( 'NONE',  ( -13.37433931291107214, 61.86190675592462185, -1.950432114993175814 ) ) ;
#15481 = EDGE_LOOP ( 'NONE', ( #4197, #8369, #16563, #10942 ) ) ;
#15482 = VERTEX_POINT ( 'NONE', #3271 ) ;
#15483 = CARTESIAN_POINT ( 'NONE',  ( 4.171729424061789260, 29.82999999999999474, 12.83926296998457239 ) ) ;
#15484 = CARTESIAN_POINT ( 'NONE',  ( 7.714727599200458030, -3.121874999999992628, -18.62499999999934985 ) ) ;
#15485 = EDGE_CURVE ( 'NONE', #13302, #17169, #1851, .T. ) ;
#15486 = CARTESIAN_POINT ( 'NONE',  ( 9.911774180940524204, 48.07459980054595405, 9.166220353908824947 ) ) ;
#15487 = CARTESIAN_POINT ( 'NONE',  ( 7.492398563130175049, 57.89939741061336775, -11.23087949929781360 ) ) ;
#15488 = CARTESIAN_POINT ( 'NONE',  ( 4.907594864777465204, 79.00300826774883944, -12.57642615738353342 ) ) ;
#15489 = CARTESIAN_POINT ( 'NONE',  ( 11.76794919243112325, 79.43000000000000682, 1.441158131103945434E-15 ) ) ;
#15490 = CARTESIAN_POINT ( 'NONE',  ( 7.731081879493610032, -5.208608120530584900E-17, -9.234192800205820006 ) ) ;
#15491 = CARTESIAN_POINT ( 'NONE',  ( -1.156690518843707549, 7.956351059191337782, 18.35912573876695930 ) ) ;
#15492 = DIRECTION ( 'NONE',  ( 1.000000000000000000, 0.000000000000000000, 0.000000000000000000 ) ) ;
#15493 = CARTESIAN_POINT ( 'NONE',  ( 11.37500000000039613, -43.74062499999988773, -4.711679271993004292 ) ) ;
#15494 = CARTESIAN_POINT ( 'NONE',  ( 2.247262830882058804, 53.76078584421372852, 13.32055735975993827 ) ) ;
#15495 = EDGE_LOOP ( 'NONE', ( #2173, #4939 ) ) ;
#15496 = DIRECTION ( 'NONE',  ( 0.000000000000000000, 0.000000000000000000, -1.000000000000000000 ) ) ;
#15497 = ORIENTED_EDGE ( 'NONE', *, *, #13672, .T. ) ;
#15498 = CARTESIAN_POINT ( 'NONE',  ( 4.331139769576483722, 67.02393676668302192, -12.79382777007953997 ) ) ;
#15499 = CARTESIAN_POINT ( 'NONE',  ( -10.21196434613299786, 34.59042564233829609, -8.829834170552652850 ) ) ;
#15500 = CARTESIAN_POINT ( 'NONE',  ( 11.37499999999960210, -82.20937499999980957, 4.711679271994918317 ) ) ;
#15501 = LINE ( 'NONE', #3413, #8046 ) ;
#15502 = CARTESIAN_POINT ( 'NONE',  ( -0.3547435831859336863, 59.66724472799371171, 13.49534119830239298 ) ) ;
#15503 = DIRECTION ( 'NONE',  ( -1.000000000000000000, -1.734723475976807094E-16, -0.000000000000000000 ) ) ;
#15504 = ADVANCED_FACE ( 'NONE', ( #7447 ), #6588, .T. ) ;
#15505 = FACE_OUTER_BOUND ( 'NONE', #10189, .T. ) ;
#15506 = CARTESIAN_POINT ( 'NONE',  ( 13.37527706476260114, 72.36600586506794741, 1.830836926929945152 ) ) ;
#15507 = CARTESIAN_POINT ( 'NONE',  ( 9.520470885617715595, 32.13000000000001677, 6.917026985038135400 ) ) ;
#15508 = CARTESIAN_POINT ( 'NONE',  ( 10.92172942406178926, 51.12999999999999545, 7.935100905948387684 ) ) ;
#15509 = CARTESIAN_POINT ( 'NONE',  ( -4.722038887560244369, 52.35004485108893846, -12.64903088714287627 ) ) ;
#15510 = CARTESIAN_POINT ( 'NONE',  ( -10.92172942406179104, 52.22999999999999687, 7.935100905948387684 ) ) ;
#15511 = CARTESIAN_POINT ( 'NONE',  ( 18.18516759496687030, 8.007293617507080796, -0.8582236110267621454 ) ) ;
#15512 = CARTESIAN_POINT ( 'NONE',  ( -7.272992578804310604, -1.620000000000001217, 10.01041549318726709 ) ) ;
#15513 = CARTESIAN_POINT ( 'NONE',  ( 0.8896506985072949458, 68.71206883159973700, 13.47799656996557438 ) ) ;
#15514 = CARTESIAN_POINT ( 'NONE',  ( -18.62500000000000000, -24.97499999999994102, -1.562973063126292555E-12 ) ) ;
#15515 = CARTESIAN_POINT ( 'NONE',  ( -8.891200544363830713E-16, 5.680000000000002380, 13.49999999999999822 ) ) ;
#15516 = CARTESIAN_POINT ( 'NONE',  ( -18.62499999999934985, -23.93437499999993889, -7.714727599200458918 ) ) ;
#15517 = CARTESIAN_POINT ( 'NONE',  ( -5.195004986271709591, 65.49223690651673735, 12.46041586375061883 ) ) ;
#15518 = CARTESIAN_POINT ( 'NONE',  ( -17.32050807568886697, 0.000000000000000000, 9.999999999999838352 ) ) ;
#15519 = PRODUCT_DEFINITION_FORMATION_WITH_SPECIFIED_SOURCE ( 'ANY', '', #4088, .NOT_KNOWN. ) ;
#15520 = CARTESIAN_POINT ( 'NONE',  ( 8.772452899675805327, 8.058014385990555084, -15.73598335365642953 ) ) ;
#15521 = CARTESIAN_POINT ( 'NONE',  ( -8.549982208541774191E-16, 24.67999999999999972, 14.19474002721660355 ) ) ;
#15522 = ORIENTED_EDGE ( 'NONE', *, *, #6458, .F. ) ;
#15523 = CARTESIAN_POINT ( 'NONE',  ( -3.636496289402155746, 33.52999999999999403, 11.19198476289190936 ) ) ;
#15524 = DIRECTION ( 'NONE',  ( -0.000000000000000000, 1.000000000000000000, -0.000000000000000000 ) ) ;
#15525 = ADVANCED_FACE ( 'NONE', ( #16966 ), #966, .T. ) ;
#15526 = CARTESIAN_POINT ( 'NONE',  ( -12.99763655697469389, 31.79961795752758036, -3.649497489147533802 ) ) ;
#15527 = CARTESIAN_POINT ( 'NONE',  ( 5.944571218590016137, 74.89675644291142476, 12.12073777988105050 ) ) ;
#15528 = B_SPLINE_CURVE_WITH_KNOTS ( 'NONE', 3,
 ( #7683, #12891, #16861, #6186, #5023, #12720 ),
 .UNSPECIFIED., .F., .F.,
 ( 4, 2, 4 ),
 ( 0.02310369341406991878, 0.02476750247080822948, 0.02643131152754654364 ),
 .UNSPECIFIED. ) ;
#15529 = CARTESIAN_POINT ( 'NONE',  ( 2.445080149700053643E-15, 63.17999999999998550, -13.50000000000000000 ) ) ;
#15530 = CARTESIAN_POINT ( 'NONE',  ( -9.520470885617717371, 33.22999999999999687, 6.917026985038133624 ) ) ;
#15531 = CARTESIAN_POINT ( 'NONE',  ( 13.23700282839715214, 51.52360258182024921, -2.651746004224825981 ) ) ;
#15532 = CARTESIAN_POINT ( 'NONE',  ( -10.85070262625603199, 38.23431805590681876, 8.033477467492103230 ) ) ;
#15533 = CARTESIAN_POINT ( 'NONE',  ( 9.828294447040992310, 36.78977993224530252, -9.257394455623087381 ) ) ;
#15534 = CARTESIAN_POINT ( 'NONE',  ( 4.711679271994911211, -27.02187499999995524, -11.37499999999960210 ) ) ;
#15535 = LINE ( 'NONE', #4520, #7151 ) ;
#15536 = ADVANCED_BREP_SHAPE_REPRESENTATION ( '', ( #3260, #16654 ), #11308 ) ;
#15537 = CARTESIAN_POINT ( 'NONE',  ( -6.079049460997783427, 77.45800250635466000, 12.05802342483350387 ) ) ;
#15538 = CARTESIAN_POINT ( 'NONE',  ( 0.8516938202833010951, 62.71062401767625261, 13.47402210528613864 ) ) ;
#15539 = CARTESIAN_POINT ( 'NONE',  ( 2.693171479753761144, 41.77698449823576254, 13.23099151030277731 ) ) ;
#15540 = CARTESIAN_POINT ( 'NONE',  ( 8.569772578347119918, 48.85117011955044575, -10.43116877877169379 ) ) ;
#15541 = CARTESIAN_POINT ( 'NONE',  ( -9.520470885617715595, 15.63000000000000433, -6.917026985038136289 ) ) ;
#15542 = EDGE_LOOP ( 'NONE', ( #10661, #1854, #1642, #12955 ) ) ;
#15543 = CARTESIAN_POINT ( 'NONE',  ( -9.520470885617717371, 63.23000000000001108, 6.917026985038133624 ) ) ;
#15544 = CARTESIAN_POINT ( 'NONE',  ( 11.37500000000000178, 7.250000000000001776, 9.531744055041752924E-13 ) ) ;
#15545 = CARTESIAN_POINT ( 'NONE',  ( 19.00000000000000711, 0.000000000000000000, -1.732050807568807027 ) ) ;
#15546 = CARTESIAN_POINT ( 'NONE',  ( 4.171729424061791924, 1.030000000000003135, -12.83926296998457239 ) ) ;
#15547 = CARTESIAN_POINT ( 'NONE',  ( 2.279995255611139653E-15, 30.18000000000001393, -12.37355403259654985 ) ) ;
#15548 = CARTESIAN_POINT ( 'NONE',  ( -6.556136581990969603, 80.93000000000003524, -10.79013235404803162 ) ) ;
#15549 = CARTESIAN_POINT ( 'NONE',  ( 18.62500000000000000, -33.29999999999991900, 1.560692158462880521E-12 ) ) ;
#15550 = CARTESIAN_POINT ( 'NONE',  ( 0.3084388608991097125, 65.69109030173645181, 13.49649039133380768 ) ) ;
#15551 = CARTESIAN_POINT ( 'NONE',  ( -4.171729424061787483, 82.32999999999999829, -12.83926296998457417 ) ) ;
#15552 = CARTESIAN_POINT ( 'NONE',  ( 3.636496289402154414, 45.82999999999999829, 11.19198476289190936 ) ) ;
#15553 = CARTESIAN_POINT ( 'NONE',  ( -13.23862237912311990, 59.02327283768620703, 2.644021597903271292 ) ) ;
#15554 = CARTESIAN_POINT ( 'NONE',  ( 13.46303184484187021, 45.39474804055323887, 1.017860785898056619 ) ) ;
#15555 = CARTESIAN_POINT ( 'NONE',  ( 10.07434941184534161, 69.77687380662450778, -8.986611288426695765 ) ) ;
#15556 = AXIS2_PLACEMENT_3D ( 'NONE', #13321, #15878, #11920 ) ;
#15557 = CARTESIAN_POINT ( 'NONE',  ( 4.216399006263609195, 80.83160784084826389, 12.82482784682136767 ) ) ;
#15558 = CARTESIAN_POINT ( 'NONE',  ( 13.48284133012123576, 30.45349738626596192, -0.6814970486944390560 ) ) ;
#15559 = EDGE_CURVE ( 'NONE', #19, #6381, #974, .T. ) ;
#15560 = CARTESIAN_POINT ( 'NONE',  ( -12.71517232650662166, 56.09383332730872951, 4.535934352837492689 ) ) ;
#15561 = CARTESIAN_POINT ( 'NONE',  ( -3.937409535744305078, 50.53842199591847617, 12.91306281124268374 ) ) ;
#15562 = CARTESIAN_POINT ( 'NONE',  ( 5.262825442084041683, 63.98957157723919664, -12.43207888071740008 ) ) ;
#15563 = CARTESIAN_POINT ( 'NONE',  ( 13.02746587078432761, 39.55632540197606772, -3.540568321141328578 ) ) ;
#15564 = VERTEX_POINT ( 'NONE', #10360 ) ;
#15565 = CARTESIAN_POINT ( 'NONE',  ( -10.51606056038198922, 61.60671756202894755, -8.470023507808827290 ) ) ;
#15566 = ORIENTED_EDGE ( 'NONE', *, *, #11319, .F. ) ;
#15567 = VERTEX_POINT ( 'NONE', #13080 ) ;
#15568 = CARTESIAN_POINT ( 'NONE',  ( -13.50000000000000000, 28.93000000000001037, -3.469446951953614189E-15 ) ) ;
#15569 = CARTESIAN_POINT ( 'NONE',  ( 18.62499999999935341, -89.45937499999983800, 7.714727599200469577 ) ) ;
#15570 = VECTOR ( 'NONE', #665, 1000.000000000000000 ) ;
#15571 = CARTESIAN_POINT ( 'NONE',  ( 10.57931356024353242, 57.74949723134712087, -8.386364294737058245 ) ) ;
#15572 = CARTESIAN_POINT ( 'NONE',  ( 2.551961531130515493, 79.08824087738575770, -13.25660889663138065 ) ) ;
#15573 = CARTESIAN_POINT ( 'NONE',  ( -3.636496289402155746, 81.53000000000000114, 11.19198476289190936 ) ) ;
#15574 = CARTESIAN_POINT ( 'NONE',  ( 10.92172942406178926, 38.12999999999999545, 7.935100905948387684 ) ) ;
#15575 = CARTESIAN_POINT ( 'NONE',  ( 12.78940066181286106, 2.734769208434739636E-15, 0.7471054272073315294 ) ) ;
#15576 = CARTESIAN_POINT ( 'NONE',  ( -1.005545769327274827E-13, 2.180000000000013927, -13.50000000000000000 ) ) ;
#15577 = FACE_OUTER_BOUND ( 'NONE', #15836, .T. ) ;
#15578 = EDGE_CURVE ( 'NONE', #6383, #8781, #6380, .T. ) ;
#15579 = CARTESIAN_POINT ( 'NONE',  ( 15.58845726811991916, 0.000000000000000000, -10.99999999999996092 ) ) ;
#15580 = CARTESIAN_POINT ( 'NONE',  ( -8.043339635996304082, -48.94374999999985931, -8.043339635997652337 ) ) ;
#15581 = AXIS2_PLACEMENT_3D ( 'NONE', #16616, #534, #791 ) ;
#15582 = CARTESIAN_POINT ( 'NONE',  ( 3.708203932499371192, 5.896025403784444840, -11.41267819554184548 ) ) ;
#15583 = CARTESIAN_POINT ( 'NONE',  ( 3.038729800852512763, 34.07073859099919844, -13.15357245918240459 ) ) ;
#15584 = ORIENTED_EDGE ( 'NONE', *, *, #5182, .T. ) ;
#15585 = DIRECTION ( 'NONE',  ( 0.000000000000000000, 0.000000000000000000, 1.000000000000000000 ) ) ;
#15586 = ORIENTED_EDGE ( 'NONE', *, *, #17236, .T. ) ;
#15587 = B_SPLINE_CURVE_WITH_KNOTS ( 'NONE', 3,
 ( #99, #2555, #4162, #14751 ),
 .UNSPECIFIED., .F., .F.,
 ( 4, 4 ),
 ( 0.008723199174958470511, 0.01636875612029860955 ),
 .UNSPECIFIED. ) ;
#15588 = CARTESIAN_POINT ( 'NONE',  ( 4.988803385412796665, 9.999999999999996447, -12.54439479535357371 ) ) ;
#15589 = CARTESIAN_POINT ( 'NONE',  ( -4.711679271993001628, -12.45312499999998757, -11.37500000000039613 ) ) ;
#15590 = CARTESIAN_POINT ( 'NONE',  ( 8.772402711158880706, 78.01830691709993459, 10.26166134156747489 ) ) ;
#15591 = CARTESIAN_POINT ( 'NONE',  ( -6.840445147067528708, 59.42702751003819372, 11.64074063870059383 ) ) ;
#15592 = DIRECTION ( 'NONE',  ( 0.000000000000000000, -1.000000000000000000, 0.000000000000000000 ) ) ;
#15593 = CARTESIAN_POINT ( 'NONE',  ( 8.523150694292391805, 72.00656199573694494, 10.47221625061583516 ) ) ;
#15594 = CARTESIAN_POINT ( 'NONE',  ( 9.520470885617715595, 29.13000000000001677, 6.917026985038135400 ) ) ;
#15595 = CARTESIAN_POINT ( 'NONE',  ( -13.50000000000000000, 52.92999999999999972, -3.306546357697853733E-15 ) ) ;
#15596 = CARTESIAN_POINT ( 'NONE',  ( -8.465209700148607297, 52.50397567740490246, -10.51791672388853094 ) ) ;
#15597 = CARTESIAN_POINT ( 'NONE',  ( 0.000000000000000000, -22.00000000000000000, 0.000000000000000000 ) ) ;
#15598 = CARTESIAN_POINT ( 'NONE',  ( 18.62499999999934630, -48.90937499999989058, 7.714727599200467800 ) ) ;
#15599 = CARTESIAN_POINT ( 'NONE',  ( -8.863294625709455588, 68.33741696991182835, 10.18396718458916972 ) ) ;
#15600 = CARTESIAN_POINT ( 'NONE',  ( -13.16986379959834252, -22.89374999999994387, -13.16986379960055054 ) ) ;
#15601 = EDGE_CURVE ( 'NONE', #11076, #3534, #922, .T. ) ;
#15602 = CARTESIAN_POINT ( 'NONE',  ( -2.138189944381240881, 5.603118577679734535, 13.49999999999999822 ) ) ;
#15603 = CARTESIAN_POINT ( 'NONE',  ( -18.62500000000064659, -9.365624999999976552, 7.714727599197335195 ) ) ;
#15604 = CARTESIAN_POINT ( 'NONE',  ( -9.115263935278322904, 65.32561837914103364, 9.970196421953582799 ) ) ;
#15605 = CARTESIAN_POINT ( 'NONE',  ( 4.988803385412796665, 9.999999999999996447, -12.54439479535357371 ) ) ;
#15606 = CARTESIAN_POINT ( 'NONE',  ( -13.49999999999999822, 3.080000000000010285, 4.386415899144235020 ) ) ;
#15607 = VERTEX_POINT ( 'NONE', #2448 ) ;
#15608 = CARTESIAN_POINT ( 'NONE',  ( -10.92172942406179104, 9.230000000000002203, 7.935100905948385908 ) ) ;
#15609 = DIRECTION ( 'NONE',  ( 0.000000000000000000, -1.000000000000000000, 0.000000000000000000 ) ) ;
#15610 = CARTESIAN_POINT ( 'NONE',  ( -13.46321216429749157, 31.89554233233273806, -0.9972219699559256023 ) ) ;
#15611 = CARTESIAN_POINT ( 'NONE',  ( 0.3528712558444254688, 74.69265864786574127, 13.50000000000789058 ) ) ;
#15612 = CARTESIAN_POINT ( 'NONE',  ( 13.49937490039810584, 60.43467020298844261, -0.1363635455224274373 ) ) ;
#15613 = DIRECTION ( 'NONE',  ( 0.000000000000000000, -1.000000000000000000, 0.000000000000000000 ) ) ;
#15614 = CARTESIAN_POINT ( 'NONE',  ( -4.171729424061791036, 76.53000000000000114, 12.83926296998457239 ) ) ;
#15615 = CARTESIAN_POINT ( 'NONE',  ( 13.33928347952357107, 51.50486127415317839, -2.136916482695208064 ) ) ;
#15616 = CARTESIAN_POINT ( 'NONE',  ( -13.26014386489534047, 38.01975955159114307, 2.545164025099730054 ) ) ;
#15617 = EDGE_CURVE ( 'NONE', #4199, #8605, #11659, .T. ) ;
#15618 = CARTESIAN_POINT ( 'NONE',  ( 10.97833218139325773, 36.72688691708130904, -7.868713784374241627 ) ) ;
#15619 = CARTESIAN_POINT ( 'NONE',  ( 4.711679271993006957, -70.72812499999983515, 11.37500000000039257 ) ) ;
#15620 = FACE_OUTER_BOUND ( 'NONE', #11882, .T. ) ;
#15621 = CARTESIAN_POINT ( 'NONE',  ( -10.50862198025424554, 77.25342995615731922, 8.475325434927029278 ) ) ;
#15622 = CARTESIAN_POINT ( 'NONE',  ( 0.4611952739691489445, 62.69658252224193262, 13.49219369441274630 ) ) ;
#15623 = CARTESIAN_POINT ( 'NONE',  ( 5.443441962766892850, 41.87725101519070137, 12.35390569854847698 ) ) ;
#15624 = CARTESIAN_POINT ( 'NONE',  ( 12.65354452320541512, 48.60108511608657267, -4.726175205520251055 ) ) ;
#15625 = CARTESIAN_POINT ( 'NONE',  ( 7.272992578804308828, 10.98000000000000576, 10.01041549318726709 ) ) ;
#15626 = ORIENTED_EDGE ( 'NONE', *, *, #6378, .T. ) ;
#15627 = CARTESIAN_POINT ( 'NONE',  ( 3.636496289402154414, 60.82999999999999829, 11.19198476289190936 ) ) ;
#15628 = CARTESIAN_POINT ( 'NONE',  ( -8.043339635996304082, 1.006250000000015854, -8.043339635997652337 ) ) ;
#15629 = CARTESIAN_POINT ( 'NONE',  ( 4.711679271993006068, -96.77812499999977547, 11.37500000000039257 ) ) ;
#15630 = CARTESIAN_POINT ( 'NONE',  ( 13.49999999999999822, -2.719999999999995310, 4.386415899144237684 ) ) ;
#15631 = CARTESIAN_POINT ( 'NONE',  ( 3.636496289402154414, 28.82999999999999474, 11.19198476289190758 ) ) ;
#15632 = CARTESIAN_POINT ( 'NONE',  ( -11.42802927807712443, 80.93000000000000682, -3.799729825766118285 ) ) ;
#15633 = CARTESIAN_POINT ( 'NONE',  ( -18.62499999999935341, -73.88437499999982094, -7.714727599200458918 ) ) ;
#15634 = CARTESIAN_POINT ( 'NONE',  ( 3.089967991614102516, 65.79111338089974481, 13.14161812284216246 ) ) ;
#15635 = CARTESIAN_POINT ( 'NONE',  ( -8.691771469529815392E-16, 77.68000000000000682, 14.19474002721660355 ) ) ;
#15636 = CARTESIAN_POINT ( 'NONE',  ( 7.272992578804308828, 48.97999999999999687, 10.01041549318726709 ) ) ;
#15637 = DIRECTION ( 'NONE',  ( 8.673617379884037937E-17, -1.000000000000000000, 0.000000000000000000 ) ) ;
#15638 = CARTESIAN_POINT ( 'NONE',  ( -13.17315977348318157, 59.03476960960914255, 2.955331265607194613 ) ) ;
#15639 = CARTESIAN_POINT ( 'NONE',  ( 11.08286227684556380, 45.13930327551472743, 7.713911292983588908 ) ) ;
#15640 = LINE ( 'NONE', #4545, #15004 ) ;
#15641 = PLANE ( 'NONE',  #11473 ) ;
#15642 = CARTESIAN_POINT ( 'NONE',  ( 13.13090800037537953, 30.54142882776130463, -3.138511609109995160 ) ) ;
#15643 = CARTESIAN_POINT ( 'NONE',  ( -13.46562334750894330, 55.89667962494186781, -0.9653598001017119623 ) ) ;
#15644 = CARTESIAN_POINT ( 'NONE',  ( -13.50529896843892708, 49.92984903237493199, 0.0002717946928634594841 ) ) ;
#15645 = CARTESIAN_POINT ( 'NONE',  ( 5.792892470351891809, 63.96933600290971356, -12.19546835734017876 ) ) ;
#15646 = CARTESIAN_POINT ( 'NONE',  ( 4.234016314587428553, 43.02776078768052059, -12.81889670191663377 ) ) ;
#15647 = CARTESIAN_POINT ( 'NONE',  ( 13.35753582573685350, 39.50047908224951243, -2.013713484790881303 ) ) ;
#15648 = ORIENTED_EDGE ( 'NONE', *, *, #381, .T. ) ;
#15649 = CARTESIAN_POINT ( 'NONE',  ( -10.10386100637092888, 61.58468400106026053, -8.953342810708111443 ) ) ;
#15650 = CARTESIAN_POINT ( 'NONE',  ( 7.272992578804311492, 5.879999999999995453, -10.01041549318726709 ) ) ;
#15651 = VERTEX_POINT ( 'NONE', #16331 ) ;
#15652 = VERTEX_POINT ( 'NONE', #2802 ) ;
#15653 = CARTESIAN_POINT ( 'NONE',  ( 4.171729424061791924, 28.03000000000000114, -12.83926296998457239 ) ) ;
#15654 = CARTESIAN_POINT ( 'NONE',  ( 13.16986379959833897, -88.41874999999980389, 13.16986379960055409 ) ) ;
#15655 = CARTESIAN_POINT ( 'NONE',  ( 12.85888199276385890, 48.28223875469849702, 4.113822437287173450 ) ) ;
#15656 = CARTESIAN_POINT ( 'NONE',  ( 3.747811303784765791, 58.04554623404083458, -12.97209066736199645 ) ) ;
#15657 = CARTESIAN_POINT ( 'NONE',  ( 2.222695906433310942, 79.10008801533618339, -13.31607093855053314 ) ) ;
#15658 = ADVANCED_FACE ( 'NONE', ( #8411 ), #1663, .F. ) ;
#15659 = CARTESIAN_POINT ( 'NONE',  ( 3.636496289402154414, 81.82999999999999829, 11.19198476289190936 ) ) ;
#15660 = CARTESIAN_POINT ( 'NONE',  ( 13.50000000000000000, 41.42999999999999972, 1.653273178848926867E-15 ) ) ;
#15661 = CARTESIAN_POINT ( 'NONE',  ( 11.76794919243112680, 82.58000000000001251, -3.823638476888993942 ) ) ;
#15662 = DIRECTION ( 'NONE',  ( 0.000000000000000000, 0.000000000000000000, 1.000000000000000000 ) ) ;
#15663 = CARTESIAN_POINT ( 'NONE',  ( 4.171729424061791924, 42.03000000000000114, -12.83926296998457239 ) ) ;
#15664 = CARTESIAN_POINT ( 'NONE',  ( -12.50000000000000000, 98.93000000000002103, 1.224646799147353059E-15 ) ) ;
#15665 = CARTESIAN_POINT ( 'NONE',  ( -9.552639591052204498E-13, -55.18749999999985079, 11.37500000000000178 ) ) ;
#15666 = AXIS2_PLACEMENT_3D ( 'NONE', #2803, #17229, #5672 ) ;
#15667 = CARTESIAN_POINT ( 'NONE',  ( 1.137810555388867773, -1.046521029022079216E-15, -11.94593600937347055 ) ) ;
#15668 = CARTESIAN_POINT ( 'NONE',  ( 0.000000000000000000, 30.93000000000001393, 0.000000000000000000 ) ) ;
#15669 = ORIENTED_EDGE ( 'NONE', *, *, #15463, .F. ) ;
#15670 = CARTESIAN_POINT ( 'NONE',  ( -8.000000000000145661, 0.000000000000000000, 17.32050807568870709 ) ) ;
#15671 = EDGE_LOOP ( 'NONE', ( #1603, #10425, #11546, #8849 ) ) ;
#15672 = CARTESIAN_POINT ( 'NONE',  ( -8.343458848123576743, 16.48000000000000753, -11.48378591275254301 ) ) ;
#15673 = CARTESIAN_POINT ( 'NONE',  ( 4.711679271994911211, -43.67187499999991473, -11.37499999999960210 ) ) ;
#15674 = CARTESIAN_POINT ( 'NONE',  ( 1.443355482025400649, 77.73190779979329079, 13.42308081186049051 ) ) ;
#15675 = CARTESIAN_POINT ( 'NONE',  ( -0.1955871059449479643, 59.67296629411183773, 13.49897230917331292 ) ) ;
#15676 = CARTESIAN_POINT ( 'NONE',  ( 7.499999999999998224, 108.9300000000000068, 9.367496997597600128 ) ) ;
#15677 = CARTESIAN_POINT ( 'NONE',  ( -16.82677684650042593, 7.170662809914419178, 13.14483242576199018 ) ) ;
#15678 = DIRECTION ( 'NONE',  ( 0.000000000000000000, 0.000000000000000000, -1.000000000000000000 ) ) ;
#15679 = MECHANICAL_DESIGN_GEOMETRIC_PRESENTATION_REPRESENTATION (  '', ( #15396 ), #5272 ) ;
#15680 = CARTESIAN_POINT ( 'NONE',  ( -8.691771469529815392E-16, 50.67999999999999261, 14.19474002721660355 ) ) ;
#15681 = CARTESIAN_POINT ( 'NONE',  ( -4.315607089656920081, 71.52482252390403517, 12.79169210638634624 ) ) ;
#15682 = DIRECTION ( 'NONE',  ( 0.000000000000000000, 0.000000000000000000, -1.000000000000000000 ) ) ;
#15683 = CARTESIAN_POINT ( 'NONE',  ( 18.85006967243204556, 7.815232008520040630, 1.645488492587892315 ) ) ;
#15684 = CARTESIAN_POINT ( 'NONE',  ( -7.714727599197335195, -88.45312499999978684, -18.62500000000064304 ) ) ;
#15685 = CARTESIAN_POINT ( 'NONE',  ( -3.364692565120436463, 68.55914111881094186, 13.08348558152368746 ) ) ;
#15686 = CARTESIAN_POINT ( 'NONE',  ( 7.714727599197338748, -13.52812499999996732, 18.62500000000063949 ) ) ;
#15687 = CARTESIAN_POINT ( 'NONE',  ( 4.349022827738643571, 55.02346064057928032, -12.78217124321885478 ) ) ;
#15688 = CARTESIAN_POINT ( 'NONE',  ( -18.62500000000064659, -59.31562499999985505, 7.714727599197335195 ) ) ;
#15689 = AXIS2_PLACEMENT_3D ( 'NONE', #12674, #6057, #2125 ) ;
#15690 = CARTESIAN_POINT ( 'NONE',  ( -8.551869864207160887, 65.35210363059799477, 10.44874323309726272 ) ) ;
#15691 = CYLINDRICAL_SURFACE ( 'NONE', #13523, 13.50000000000000000 ) ;
#15692 = CARTESIAN_POINT ( 'NONE',  ( -3.309329455300976441, 35.56117355828821047, 13.09820044315392629 ) ) ;
#15693 = ORIENTED_EDGE ( 'NONE', *, *, #15485, .T. ) ;
#15694 = CARTESIAN_POINT ( 'NONE',  ( 9.520470885617715595, 31.12999999999999901, 6.917026985038134512 ) ) ;
#15695 = LINE ( 'NONE', #14035, #4648 ) ;
#15696 = CARTESIAN_POINT ( 'NONE',  ( -4.945118968609875765, 40.35832260886622436, -12.56369513011831174 ) ) ;
#15697 = CARTESIAN_POINT ( 'NONE',  ( -11.82971441149514469, 31.68901184113946812, -6.504453626418047918 ) ) ;
#15698 = DIRECTION ( 'NONE',  ( 1.000000000000000000, 0.000000000000000000, 6.313931023057710304E-15 ) ) ;
#15699 = CARTESIAN_POINT ( 'NONE',  ( 10.65864953284609129, 60.11494968480803891, 8.285120799684273507 ) ) ;
#15700 = EDGE_CURVE ( 'NONE', #7488, #10745, #3073, .T. ) ;
#15701 = CARTESIAN_POINT ( 'NONE',  ( -13.50000000000000000, 5.930000000000005045, -3.469446951953614189E-15 ) ) ;
#15702 = EDGE_CURVE ( 'NONE', #8166, #14419, #10816, .T. ) ;
#15703 = CARTESIAN_POINT ( 'NONE',  ( 2.138189944381238661, 2.756881422320272002, 13.49999999999999822 ) ) ;
#15704 = CARTESIAN_POINT ( 'NONE',  ( -3.636496289402153081, 62.32999999999999829, -11.19198476289190936 ) ) ;
#15705 = CARTESIAN_POINT ( 'NONE',  ( 10.92172942406179104, 71.73000000000000398, -7.935100905948385908 ) ) ;
#15706 = CARTESIAN_POINT ( 'NONE',  ( 13.40485122747304914, 51.37422532693715027, 1.600017051684848202 ) ) ;
#15707 =( BOUNDED_CURVE ( )  B_SPLINE_CURVE ( 2, ( #14928, #1676, #101, #2820, #4434, #12298, #8249, #192, #5597, #10978, #16349, #4255, #9664 ),
 .UNSPECIFIED., .F., .F. ) 
 B_SPLINE_CURVE_WITH_KNOTS ( ( 3, 2, 2, 2, 2, 2, 3 ),
 ( 0.4861111111111111049, 0.4888888888888888729, 0.4944444444444444642, 0.5000000000000000000, 0.5055555555555555358, 0.5111111111111110716, 0.5138888888888888395 ),
 .UNSPECIFIED. ) 
 CURVE ( )  GEOMETRIC_REPRESENTATION_ITEM ( )  RATIONAL_B_SPLINE_CURVE ( ( 0.9755282581475768211, 0.9755282581475768211, 1.000000000000000000, 0.9510565162951535312, 1.000000000000000000, 0.9510565162951535312, 1.000000000000000000, 0.9510565162951535312, 1.000000000000000000, 0.9510565162951535312, 1.000000000000000000, 0.9755282581475772652, 0.9755282581475768211 ) ) 
 REPRESENTATION_ITEM ( '' )  );
#15708 = CARTESIAN_POINT ( 'NONE',  ( -13.47842577702374278, 37.96032382249477877, 0.8798576433466377411 ) ) ;
#15709 = CARTESIAN_POINT ( 'NONE',  ( 13.17094745865578709, 36.53536659866002623, -2.974084169080610796 ) ) ;
#15710 = CARTESIAN_POINT ( 'NONE',  ( -11.37499999999960210, -14.53437499999998295, -4.711679271994911211 ) ) ;
#15711 = CARTESIAN_POINT ( 'NONE',  ( -5.620096583852075334, 74.47603443507840382, 12.27847533565288884 ) ) ;
#15712 = CARTESIAN_POINT ( 'NONE',  ( -3.551554394246068558, 77.55229557867063761, 13.02528201803605512 ) ) ;
#15713 = CARTESIAN_POINT ( 'NONE',  ( -10.92172942406178926, 60.63000000000000256, -7.935100905948389460 ) ) ;
#15714 = CARTESIAN_POINT ( 'NONE',  ( 7.500000000000000888, 102.9300000000000068, -9.367496997597600128 ) ) ;
#15715 = ORIENTED_EDGE ( 'NONE', *, *, #11084, .T. ) ;
#15716 = CARTESIAN_POINT ( 'NONE',  ( -11.76794919243112325, 10.08000000000000718, 3.823638476888994386 ) ) ;
#15717 = ORIENTED_EDGE ( 'NONE', *, *, #14092, .T. ) ;
#15718 = CARTESIAN_POINT ( 'NONE',  ( 11.76794919243112325, 58.28000000000000114, 3.823638476888997051 ) ) ;
#15719 = CARTESIAN_POINT ( 'NONE',  ( -11.37499999999960743, -83.28437499999976978, -4.711679271994912099 ) ) ;
#15720 = CARTESIAN_POINT ( 'NONE',  ( 12.50000000000000000, 102.9300000000000210, 1.714505518806294638E-15 ) ) ;
#15721 = CARTESIAN_POINT ( 'NONE',  ( 6.659136588377341681, 75.93459917958982430, -11.75290894059296853 ) ) ;
#15722 = ADVANCED_FACE ( 'NONE', ( #1576 ), #6994, .F. ) ;
#15723 = CARTESIAN_POINT ( 'NONE',  ( 1.561832610794586538E-12, -37.46249999999991331, -18.62500000000000000 ) ) ;
#15724 = CARTESIAN_POINT ( 'NONE',  ( -2.970370385949294256, 7.170662809914418290, -21.14483242576214295 ) ) ;
#15725 = CARTESIAN_POINT ( 'NONE',  ( -7.272992578804310604, 48.38000000000000256, 10.01041549318726709 ) ) ;
#15726 = CARTESIAN_POINT ( 'NONE',  ( -11.88920123096388792, 9.999999999999994671, -1.626927807140451154 ) ) ;
#15727 = CARTESIAN_POINT ( 'NONE',  ( -13.45261086486871172, 58.96929453956708045, 1.133742953798396291 ) ) ;
#15728 = CARTESIAN_POINT ( 'NONE',  ( 11.63529875998058927, 45.17511335439066045, 6.848266737798307524 ) ) ;
#15729 = CARTESIAN_POINT ( 'NONE',  ( 12.82150868624539086, 69.27794690079218753, 4.225997539185415874 ) ) ;
#15730 = DIRECTION ( 'NONE',  ( 0.000000000000000000, 0.000000000000000000, -1.000000000000000000 ) ) ;
#15731 = CARTESIAN_POINT ( 'NONE',  ( 12.09037112244008405, 30.65106581466645608, -6.006992855518931584 ) ) ;
#15732 = CARTESIAN_POINT ( 'NONE',  ( -9.995403852311815385, 55.57895733551523421, -9.074982918291022216 ) ) ;
#15733 = CARTESIAN_POINT ( 'NONE',  ( -11.01017756159927785, 50.22480640622728032, 7.811931653475178372 ) ) ;
#15734 = CARTESIAN_POINT ( 'NONE',  ( 5.199860282695291325, 63.99191061641860756, -12.45850863233871486 ) ) ;
#15735 = CARTESIAN_POINT ( 'NONE',  ( 24.73863375370599016, 5.918584287042170544, -7.999999999999936051 ) ) ;
#15736 = CARTESIAN_POINT ( 'NONE',  ( 13.31623920422783591, 39.35204567939386777, 2.219880403359409282 ) ) ;
#15737 = ORIENTED_EDGE ( 'NONE', *, *, #7763, .F. ) ;
#15738 = CARTESIAN_POINT ( 'NONE',  ( -10.11420833265737507, 70.58488754181632885, -8.944704958495304226 ) ) ;
#15739 = CARTESIAN_POINT ( 'NONE',  ( -4.072279632042837605, 61.32642407186975930, -12.87115663778308061 ) ) ;
#15740 = CARTESIAN_POINT ( 'NONE',  ( 3.636496289402154414, 4.830000000000000959, 11.19198476289190758 ) ) ;
#15741 = ORIENTED_EDGE ( 'NONE', *, *, #14797, .T. ) ;
#15742 = CARTESIAN_POINT ( 'NONE',  ( -11.83065338684570911, 40.68906663066565699, -6.503147009567541659 ) ) ;
#15743 = ORIENTED_EDGE ( 'NONE', *, *, #10854, .T. ) ;
#15744 = CARTESIAN_POINT ( 'NONE',  ( -10.92172942406179104, 20.22999999999999687, 7.935100905948385908 ) ) ;
#15745 = CARTESIAN_POINT ( 'NONE',  ( -7.714727599197334307, -95.70312499999980105, -18.62500000000064659 ) ) ;
#15746 = CARTESIAN_POINT ( 'NONE',  ( 2.636929751653812382, 47.77487479848526419, 13.24312322384484020 ) ) ;
#15747 = EDGE_CURVE ( 'NONE', #13897, #14419, #4028, .T. ) ;
#15748 = CARTESIAN_POINT ( 'NONE',  ( 7.843744172734761655, 57.88406826092607815, -10.98845944672378394 ) ) ;
#15749 = CARTESIAN_POINT ( 'NONE',  ( 12.19393943590524998, 78.64260903952070692, -5.792913002744612960 ) ) ;
#15750 = CARTESIAN_POINT ( 'NONE',  ( 7.272992578804311492, 82.87999999999999545, -10.01041549318726709 ) ) ;
#15751 = CARTESIAN_POINT ( 'NONE',  ( 12.44496325052851127, -3.033844236144862824E-15, -2.130170732896519148 ) ) ;
#15752 = FACE_OUTER_BOUND ( 'NONE', #2236, .T. ) ;
#15753 = AXIS2_PLACEMENT_3D ( 'NONE', #9817, #6985, #14990 ) ;
#15754 = CARTESIAN_POINT ( 'NONE',  ( 9.073745536650823951, -100.0000000000000995, 7.819101196815612553 ) ) ;
#15755 = CARTESIAN_POINT ( 'NONE',  ( -0.06858017979864573788, 67.18246588477448711, -13.49985044511317334 ) ) ;
#15756 = CARTESIAN_POINT ( 'NONE',  ( -9.552639591052204498E-13, -21.88749999999992824, 11.37500000000000178 ) ) ;
#15757 = CARTESIAN_POINT ( 'NONE',  ( 13.50000000000000355, 44.57999999999999829, -4.386415899144233244 ) ) ;
#15758 = CARTESIAN_POINT ( 'NONE',  ( 0.5908221627133811715, 34.15875621469567847, -13.50000000000000355 ) ) ;
#15759 = CARTESIAN_POINT ( 'NONE',  ( -13.50303335837387309, 73.92924155917964413, -0.01907866586608939624 ) ) ;
#15760 = ORIENTED_EDGE ( 'NONE', *, *, #6458, .T. ) ;
#15761 = DIRECTION ( 'NONE',  ( 1.000000000000000000, 0.000000000000000000, 0.000000000000000000 ) ) ;
#15762 = ORIENTED_EDGE ( 'NONE', *, *, #16745, .F. ) ;
#15763 = CARTESIAN_POINT ( 'NONE',  ( 10.92172942406178926, 15.13000000000000433, 7.935100905948385908 ) ) ;
#15764 = CARTESIAN_POINT ( 'NONE',  ( -8.043339635997654113, -77.00624999999982379, 8.043339635996302306 ) ) ;
#15765 = AXIS2_PLACEMENT_3D ( 'NONE', #8597, #619, #12561 ) ;
#15766 = LINE ( 'NONE', #14787, #17344 ) ;
#15767 = CARTESIAN_POINT ( 'NONE',  ( -7.298493437496628822, 59.40772321095889907, 11.35718403328393755 ) ) ;
#15768 = DIRECTION ( 'NONE',  ( 0.000000000000000000, 1.000000000000000000, 0.000000000000000000 ) ) ;
#15769 = DIRECTION ( 'NONE',  ( 1.000000000000000000, -0.000000000000000000, 1.224646799147353207E-16 ) ) ;
#15770 = CARTESIAN_POINT ( 'NONE',  ( -13.49999999999999822, 52.77999999999998693, -4.386415899144240349 ) ) ;
#15771 = CARTESIAN_POINT ( 'NONE',  ( -3.576470617035913513, 71.55150969693022489, 13.02043708789197218 ) ) ;
#15772 = AXIS2_PLACEMENT_3D ( 'NONE', #4254, #191, #15014 ) ;
#15773 = CARTESIAN_POINT ( 'NONE',  ( 18.62500000000000000, -49.94999999999988205, 1.560692158462880521E-12 ) ) ;
#15774 = CARTESIAN_POINT ( 'NONE',  ( -5.119445439576221446, 68.49501675060221828, 12.49523006263062008 ) ) ;
#15775 = CARTESIAN_POINT ( 'NONE',  ( -13.16986379959834252, -72.84374999999981526, -13.16986379960055054 ) ) ;
#15776 = CARTESIAN_POINT ( 'NONE',  ( 6.029514697490034436, 54.95989846906334009, -12.07890518949519709 ) ) ;
#15777 = CARTESIAN_POINT ( 'NONE',  ( 2.279995255611139653E-15, 21.17999999999998906, -12.37355403259654985 ) ) ;
#15778 = CARTESIAN_POINT ( 'NONE',  ( -18.62499999999934985, -40.58437499999990905, -7.714727599200458918 ) ) ;
#15779 = ADVANCED_FACE ( 'NONE', ( #8499 ), #16512, .F. ) ;
#15780 = CARTESIAN_POINT ( 'NONE',  ( -2.542243399751729083, 65.58859028378583389, 13.25847602317422869 ) ) ;
#15781 = FACE_OUTER_BOUND ( 'NONE', #13620, .T. ) ;
#15782 = AXIS2_PLACEMENT_3D ( 'NONE', #843, #15503, #2243 ) ;
#15783 = CARTESIAN_POINT ( 'NONE',  ( -10.44753565030824305, 35.25738875665259542, 8.561908802029048360 ) ) ;
#15784 = CARTESIAN_POINT ( 'NONE',  ( 8.343458848123583849, 22.88000000000001322, -11.48378591275253768 ) ) ;
#15785 = ORIENTED_EDGE ( 'NONE', *, *, #10879, .F. ) ;
#15786 = DIRECTION ( 'NONE',  ( -0.000000000000000000, -1.000000000000000000, -0.000000000000000000 ) ) ;
#15787 = DIRECTION ( 'NONE',  ( 0.000000000000000000, 0.000000000000000000, -1.000000000000000000 ) ) ;
#15788 = CARTESIAN_POINT ( 'NONE',  ( -1.117267249152343211, 40.22013350474495752, -13.46142176141221114 ) ) ;
#15789 = CARTESIAN_POINT ( 'NONE',  ( -12.64316203278966455, 32.10137934669921833, 4.733190063705147388 ) ) ;
#15790 = PLANE ( 'NONE',  #14709 ) ;
#15791 = CARTESIAN_POINT ( 'NONE',  ( 10.70269728238857532, 60.11743682513120035, 8.228172719481563036 ) ) ;
#15792 = CARTESIAN_POINT ( 'NONE',  ( 4.171729424061789260, -11.16999999999999993, 12.83926296998457239 ) ) ;
#15793 = CARTESIAN_POINT ( 'NONE',  ( -10.56096607446065683, 53.25065828476769525, 8.412065287595915208 ) ) ;
#15794 = CARTESIAN_POINT ( 'NONE',  ( 7.272992578804311492, 55.87999999999998835, -10.01041549318726709 ) ) ;
#15795 = CARTESIAN_POINT ( 'NONE',  ( -8.343458848123576743, 75.48000000000001819, -11.48378591275254301 ) ) ;
#15796 = CARTESIAN_POINT ( 'NONE',  ( 13.48614702091186679, 51.45107933675966905, -0.6119089703848084039 ) ) ;
#15797 = CARTESIAN_POINT ( 'NONE',  ( -8.740153168478604684, 38.34338314764683275, 10.29122014725719758 ) ) ;
#15798 = AXIS2_PLACEMENT_3D ( 'NONE', #7349, #11843, #16055 ) ;
#15799 = CARTESIAN_POINT ( 'NONE',  ( 10.35803651828807048, 36.76167587533018377, -8.658012760942717989 ) ) ;
#15800 = CARTESIAN_POINT ( 'NONE',  ( -4.711679271993001628, -79.05312499999985221, -11.37500000000039613 ) ) ;
#15801 = EDGE_CURVE ( 'NONE', #10721, #3211, #16782, .T. ) ;
#15802 = CARTESIAN_POINT ( 'NONE',  ( -5.011838315114361286, 74.49902066430979630, 12.53603190239770271 ) ) ;
#15803 = CARTESIAN_POINT ( 'NONE',  ( -10.15729662139356471, 77.27267320848328325, 8.903693602875414115 ) ) ;
#15804 = CARTESIAN_POINT ( 'NONE',  ( -6.538465195716074874, 80.43943283378160913, 11.81155471837914384 ) ) ;
#15805 = DIRECTION ( 'NONE',  ( 0.000000000000000000, 1.000000000000000000, 0.000000000000000000 ) ) ;
#15806 = ORIENTED_EDGE ( 'NONE', *, *, #14287, .F. ) ;
#15807 = CARTESIAN_POINT ( 'NONE',  ( 2.279995255611139653E-15, 9.179999999999992610, -12.37355403259654985 ) ) ;
#15808 = ORIENTED_EDGE ( 'NONE', *, *, #5942, .F. ) ;
#15809 = CARTESIAN_POINT ( 'NONE',  ( 3.636496289402154414, 57.82999999999999829, 11.19198476289190936 ) ) ;
#15810 = CARTESIAN_POINT ( 'NONE',  ( 4.711679271994911211, -79.12187499999980389, -11.37499999999960743 ) ) ;
#15811 = CYLINDRICAL_SURFACE ( 'NONE', #3717, 13.50000000000000000 ) ;
#15812 = CARTESIAN_POINT ( 'NONE',  ( 10.92172942406179104, -2.269999999999994245, -7.935100905948385908 ) ) ;
#15813 = CARTESIAN_POINT ( 'NONE',  ( 3.698094387297103047, 76.04702867827543855, -12.98363822668122758 ) ) ;
#15814 = CARTESIAN_POINT ( 'NONE',  ( 10.92172942406178926, 32.12999999999999545, 7.935100905948387684 ) ) ;
#15815 = CARTESIAN_POINT ( 'NONE',  ( -10.92172942406179104, 77.23000000000000398, 7.935100905948387684 ) ) ;
#15816 =( BOUNDED_CURVE ( )  B_SPLINE_CURVE ( 2, ( #13539, #1428, #16632, #15112, #9857, #12313, #5612, #13626, #12578, #7108, #207, #11169, #291 ),
 .UNSPECIFIED., .F., .F. ) 
 B_SPLINE_CURVE_WITH_KNOTS ( ( 3, 2, 2, 2, 2, 2, 3 ),
 ( 0.4861111111111111049, 0.4888888888888888729, 0.4944444444444444642, 0.5000000000000000000, 0.5055555555555555358, 0.5111111111111110716, 0.5138888888888888395 ),
 .UNSPECIFIED. ) 
 CURVE ( )  GEOMETRIC_REPRESENTATION_ITEM ( )  RATIONAL_B_SPLINE_CURVE ( ( 0.9755282581475768211, 0.9755282581475768211, 1.000000000000000000, 0.9510565162951535312, 1.000000000000000000, 0.9510565162951535312, 1.000000000000000000, 0.9510565162951535312, 1.000000000000000000, 0.9510565162951535312, 1.000000000000000000, 0.9755282581475772652, 0.9755282581475768211 ) ) 
 REPRESENTATION_ITEM ( '' )  );
#15817 = CARTESIAN_POINT ( 'NONE',  ( 11.76794919243112325, 43.42999999999999972, 1.441158131103945434E-15 ) ) ;
#15818 = DIRECTION ( 'NONE',  ( 0.000000000000000000, 0.000000000000000000, -1.000000000000000000 ) ) ;
#15819 = CARTESIAN_POINT ( 'NONE',  ( -13.46128659113321113, 58.89463545154691104, -1.023806176390480438 ) ) ;
#15820 = CARTESIAN_POINT ( 'NONE',  ( 12.94169128974424510, 45.29239941246957812, 3.842414863143926329 ) ) ;
#15821 = CARTESIAN_POINT ( 'NONE',  ( 12.14869877942370735, 69.64635006548208196, -5.889954931317291198 ) ) ;
#15822 = CARTESIAN_POINT ( 'NONE',  ( -10.92172942406179104, 67.23000000000000398, 7.935100905948387684 ) ) ;
#15823 = CARTESIAN_POINT ( 'NONE',  ( 12.09463382724336000, 30.20907098269022484, 6.000288655847534791 ) ) ;
#15824 = CARTESIAN_POINT ( 'NONE',  ( -7.477981820817456438, 55.45997926997171845, -11.23979076186452453 ) ) ;
#15825 = EDGE_CURVE ( 'NONE', #9583, #12239, #7718, .T. ) ;
#15826 = CARTESIAN_POINT ( 'NONE',  ( -10.19986417753999142, 50.27059177842374993, 8.854060500917482202 ) ) ;
#15827 = CARTESIAN_POINT ( 'NONE',  ( 7.977012331873297946, 63.87814718858143692, -10.89160525889778519 ) ) ;
#15828 = CARTESIAN_POINT ( 'NONE',  ( 10.25680675266404585, 42.76715089671812819, -8.777717763810738205 ) ) ;
#15829 = CARTESIAN_POINT ( 'NONE',  ( 12.47371269042021780, 39.24203742358702840, 5.163095893957874161 ) ) ;
#15830 = ORIENTED_EDGE ( 'NONE', *, *, #14946, .F. ) ;
#15831 = CARTESIAN_POINT ( 'NONE',  ( -7.882982835668106425, 70.47768290884718567, -10.95958355943866991 ) ) ;
#15832 = CARTESIAN_POINT ( 'NONE',  ( -11.20375019216649903, 61.64692594173555307, -7.531763781615398834 ) ) ;
#15833 = CARTESIAN_POINT ( 'NONE',  ( -11.76794919243112325, 6.930000000000005933, -2.602085213965210642E-15 ) ) ;
#15834 = ORIENTED_EDGE ( 'NONE', *, *, #277, .F. ) ;
#15835 = CARTESIAN_POINT ( 'NONE',  ( -6.490606702026376240, 40.41856083592690396, -11.84311563964773306 ) ) ;
#15836 = EDGE_LOOP ( 'NONE', ( #9891, #12830, #4109, #1101 ) ) ;
#15837 = CARTESIAN_POINT ( 'NONE',  ( -13.49999999999999822, 26.08000000000000895, 4.386415899144235908 ) ) ;
#15838 = DIRECTION ( 'NONE',  ( -0.000000000000000000, -1.000000000000000000, -0.000000000000000000 ) ) ;
#15839 = CARTESIAN_POINT ( 'NONE',  ( -5.281055406448098636E-10, 61.18000001472334759, -13.50000000000000000 ) ) ;
#15840 = CARTESIAN_POINT ( 'NONE',  ( 13.49150116428843837, 57.44702109627492348, -0.4955463281862768077 ) ) ;
#15841 = CARTESIAN_POINT ( 'NONE',  ( 7.272992578804311492, 76.88000000000000966, -10.01041549318726709 ) ) ;
#15842 = CARTESIAN_POINT ( 'NONE',  ( 3.636496289402157078, 80.03000000000000114, -11.19198476289190936 ) ) ;
#15843 = AXIS2_PLACEMENT_3D ( 'NONE', #15289, #8612, #6213 ) ;
#15844 = CARTESIAN_POINT ( 'NONE',  ( -0.3356469398848770380, 47.66793158906188665, 13.49583837495916505 ) ) ;
#15845 = CARTESIAN_POINT ( 'NONE',  ( 5.665088118870674982, -100.0000000000000000, 11.78543286343676044 ) ) ;
#15846 = LINE ( 'NONE', #3753, #5448 ) ;
#15847 = CARTESIAN_POINT ( 'NONE',  ( -9.552639591052204498E-13, -71.83749999999979252, 11.37500000000000178 ) ) ;
#15848 = ADVANCED_FACE ( 'NONE', ( #521 ), #8586, .T. ) ;
#15849 = CARTESIAN_POINT ( 'NONE',  ( 13.49999999999999822, 44.27999999999999403, 4.386415899144236796 ) ) ;
#15850 = CARTESIAN_POINT ( 'NONE',  ( 7.682691750080786086, 33.89118886932563157, -11.10494913091865143 ) ) ;
#15851 = CARTESIAN_POINT ( 'NONE',  ( -2.307751883485523514, 73.26297825885289683, -13.30128957637999321 ) ) ;
#15852 = VERTEX_POINT ( 'NONE', #10000 ) ;
#15853 = ORIENTED_EDGE ( 'NONE', *, *, #16431, .T. ) ;
#15854 = CARTESIAN_POINT ( 'NONE',  ( 3.636496289402154414, 75.83000000000001251, 11.19198476289190936 ) ) ;
#15855 = ORIENTED_EDGE ( 'NONE', *, *, #6829, .F. ) ;
#15856 = AXIS2_PLACEMENT_3D ( 'NONE', #6678, #13209, #9167 ) ;
#15857 = CARTESIAN_POINT ( 'NONE',  ( 10.92172942406179104, 12.73000000000001819, -7.935100905948385908 ) ) ;
#15858 = CARTESIAN_POINT ( 'NONE',  ( 11.37499999999960210, -56.15937499999989058, 4.711679271994916540 ) ) ;
#15859 = CARTESIAN_POINT ( 'NONE',  ( -7.427281423385845294, 44.40220115185869076, 11.27323933198727346 ) ) ;
#15860 = CARTESIAN_POINT ( 'NONE',  ( -7.499999999999993783, -27.17584396961776250, -5.080312676971237451 ) ) ;
#15861 = CARTESIAN_POINT ( 'NONE',  ( 11.67414954186575926, 66.68222205810447178, -6.779902939383848803 ) ) ;
#15862 = CARTESIAN_POINT ( 'NONE',  ( -10.92172942406179104, 50.22999999999999687, 7.935100905948387684 ) ) ;
#15863 = CARTESIAN_POINT ( 'NONE',  ( -8.195680094490986889, 71.36831669863111927, 10.72758201758851548 ) ) ;
#15864 = AXIS2_PLACEMENT_3D ( 'NONE', #2981, #4147, #11138 ) ;
#15865 = CARTESIAN_POINT ( 'NONE',  ( -7.714727599200466912, -4.196874999999971934, 18.62499999999935341 ) ) ;
#15866 = CARTESIAN_POINT ( 'NONE',  ( -13.21120980875378059, 68.02931360559055918, 2.809030978660246536 ) ) ;
#15867 = CARTESIAN_POINT ( 'NONE',  ( 7.714727599197338748, -80.12812499999981242, 18.62500000000063949 ) ) ;
#15868 = CARTESIAN_POINT ( 'NONE',  ( 8.760382117191685580, 54.84251356804755773, -10.27401743239077803 ) ) ;
#15869 = CARTESIAN_POINT ( 'NONE',  ( -7.409984580736203970E-16, 19.68000000000001393, 12.37355403259654985 ) ) ;
#15870 = CARTESIAN_POINT ( 'NONE',  ( 13.16986379959834075, -64.51874999999984084, 13.16986379960055231 ) ) ;
#15871 = CARTESIAN_POINT ( 'NONE',  ( -11.50829892323420012, 65.19348115225962204, 7.057553676268226717 ) ) ;
#15872 = CARTESIAN_POINT ( 'NONE',  ( -1.703947211885682211, 62.61875151748889579, 13.39354096409387118 ) ) ;
#15873 = CARTESIAN_POINT ( 'NONE',  ( -11.31049946513870275, 35.20637627411365855, 7.370616573443121489 ) ) ;
#15874 = CARTESIAN_POINT ( 'NONE',  ( 10.92172942406178926, 19.13000000000000966, 7.935100905948385908 ) ) ;
#15875 = CARTESIAN_POINT ( 'NONE',  ( -10.92172942406178926, 8.629999999999999005, -7.935100905948389460 ) ) ;
#15876 = AXIS2_PLACEMENT_3D ( 'NONE', #8998, #6090, #7672 ) ;
#15877 = CARTESIAN_POINT ( 'NONE',  ( -13.45890448833404207, 31.89355665744642820, -1.054546249422317450 ) ) ;
#15878 = DIRECTION ( 'NONE',  ( -0.000000000000000000, -1.000000000000000000, -0.000000000000000000 ) ) ;
#15879 = CARTESIAN_POINT ( 'NONE',  ( 11.08453223446139368, 60.13957240781945046, 7.713806355306156881 ) ) ;
#15880 = CARTESIAN_POINT ( 'NONE',  ( -3.154868868512232361, 53.56660037773436045, 13.12768685552039472 ) ) ;
#15881 = EDGE_CURVE ( 'NONE', #10678, #10403, #12222, .T. ) ;
#15882 = CARTESIAN_POINT ( 'NONE',  ( -7.272992578804310604, 57.37999999999998835, 10.01041549318726709 ) ) ;
#15883 = CARTESIAN_POINT ( 'NONE',  ( 13.50000000000000000, 74.42999999999999261, 1.653273178848926867E-15 ) ) ;
#15884 = CARTESIAN_POINT ( 'NONE',  ( 6.847475264325973754, 50.93311729376924291, 11.64706806883375734 ) ) ;
#15885 = CARTESIAN_POINT ( 'NONE',  ( -11.21746825162109751, 38.21221880008548766, 7.511220640065156218 ) ) ;
#15886 = CARTESIAN_POINT ( 'NONE',  ( 11.29157302505232430, 36.70761492676916049, -7.399503251687141514 ) ) ;
#15887 = CARTESIAN_POINT ( 'NONE',  ( -9.552639591052204498E-13, -19.73749999999997229, 11.37499999999999645 ) ) ;
#15888 = CARTESIAN_POINT ( 'NONE',  ( 1.732050807568740858, 0.000000000000000000, 19.00000000000000355 ) ) ;
#15889 = CARTESIAN_POINT ( 'NONE',  ( -12.15072432148234327, 77.14617109779081261, 5.883034232685984577 ) ) ;
#15890 = CARTESIAN_POINT ( 'NONE',  ( -7.867136275643527021, 80.38330200039787599, 10.97981010490558695 ) ) ;
#15891 = CARTESIAN_POINT ( 'NONE',  ( -11.76794919243112325, 9.780000000000002913, -3.823638476888998827 ) ) ;
#15892 = CARTESIAN_POINT ( 'NONE',  ( 7.500000000000000000, 106.0143933292129361, 8.253836299850743075 ) ) ;
#15893 = EDGE_LOOP ( 'NONE', ( #5645, #14438, #7490, #5463, #5169, #4021 ) ) ;
#15894 = CARTESIAN_POINT ( 'NONE',  ( 12.50000000000000000, -18.00000000000000355, 8.999999999999998224 ) ) ;
#15895 = CARTESIAN_POINT ( 'NONE',  ( 3.636496289402154414, 16.83000000000001251, 11.19198476289190758 ) ) ;
#15896 = ORIENTED_EDGE ( 'NONE', *, *, #11479, .F. ) ;
#15897 = CARTESIAN_POINT ( 'NONE',  ( -7.272992578804307939, 56.47999999999998977, -10.01041549318727064 ) ) ;
#15898 = CARTESIAN_POINT ( 'NONE',  ( 11.37500000000000178, -92.64999999999974989, 9.531744055041752924E-13 ) ) ;
#15899 = CARTESIAN_POINT ( 'NONE',  ( -13.49999999999999822, -7.220000000000005969, -4.386415899144240349 ) ) ;
#15900 = CARTESIAN_POINT ( 'NONE',  ( 6.254386305572761096, 75.95091365744046641, -11.96381775906021794 ) ) ;
#15901 = CARTESIAN_POINT ( 'NONE',  ( 10.92172942406179104, 32.72999999999999687, -7.935100905948385908 ) ) ;
#15902 = CARTESIAN_POINT ( 'NONE',  ( 10.92172942406179104, 72.73000000000000398, -7.935100905948385908 ) ) ;
#15903 = CARTESIAN_POINT ( 'NONE',  ( 7.272992578804311492, 40.87999999999998835, -10.01041549318726709 ) ) ;
#15904 = PLANE ( 'NONE',  #4108 ) ;
#15905 = CARTESIAN_POINT ( 'NONE',  ( -10.88971337417516949, 59.23191255126531729, 7.979255671233033809 ) ) ;
#15906 = CARTESIAN_POINT ( 'NONE',  ( 7.730634896388627553, 44.97100470643064796, 11.07641855958759969 ) ) ;
#15907 = CARTESIAN_POINT ( 'NONE',  ( 12.81778580762176922, 69.27751987638765740, 4.237276121753580149 ) ) ;
#15908 = CARTESIAN_POINT ( 'NONE',  ( -13.49999999999999822, 67.07999999999999829, 4.386415899144235020 ) ) ;
#15909 = CARTESIAN_POINT ( 'NONE',  ( -12.00000000000000355, 4.213974596215569690, 3.899036354794875425 ) ) ;
#15910 = CARTESIAN_POINT ( 'NONE',  ( -10.09420973937047172, 55.58417831355667715, -8.964204995116103802 ) ) ;
#15911 = CARTESIAN_POINT ( 'NONE',  ( -11.02125367826103997, 50.22414744263306829, 7.796281688550792843 ) ) ;
#15912 = CARTESIAN_POINT ( 'NONE',  ( 2.375566496671534189, 64.09458955305812822, -13.29290925995572792 ) ) ;
#15913 = CARTESIAN_POINT ( 'NONE',  ( 11.92353461362217537, 42.66400819043492021, -6.330823637012009009 ) ) ;
#15914 = CARTESIAN_POINT ( 'NONE',  ( 12.51114643976912433, 39.24558153982501807, 5.071609117201407280 ) ) ;
#15915 = VERTEX_POINT ( 'NONE', #4766 ) ;
#15916 = CARTESIAN_POINT ( 'NONE',  ( -5.474767670627016081, 70.37845246078859418, -12.34033127765731486 ) ) ;
#15917 = CARTESIAN_POINT ( 'NONE',  ( -11.14440460645358577, 61.64327494009675235, -7.619238717130787819 ) ) ;
#15918 = CARTESIAN_POINT ( 'NONE',  ( 2.279995255611139653E-15, 3.180000000000006821, -12.37355403259654985 ) ) ;
#15919 = ORIENTED_EDGE ( 'NONE', *, *, #17109, .F. ) ;
#15920 = AXIS2_PLACEMENT_3D ( 'NONE', #763, #4831, #14353 ) ;
#15921 = EDGE_LOOP ( 'NONE', ( #5079, #10476, #16196, #13236 ) ) ;
#15922 = CARTESIAN_POINT ( 'NONE',  ( 13.49999999999999822, 24.28000000000001180, 4.386415899144237684 ) ) ;
#15923 = CARTESIAN_POINT ( 'NONE',  ( 13.16986379960055054, -68.68124999999983515, -13.16986379959834430 ) ) ;
#15924 = CARTESIAN_POINT ( 'NONE',  ( 3.064866251608231007, 61.06979871462648646, -13.14749468302701807 ) ) ;
#15925 = CARTESIAN_POINT ( 'NONE',  ( 13.32344742245652292, 57.50688615378314950, -2.187503503881035538 ) ) ;
#15926 = CARTESIAN_POINT ( 'NONE',  ( 3.636496289402154414, 69.82999999999999829, 11.19198476289190936 ) ) ;
#15927 = B_SPLINE_CURVE_WITH_KNOTS ( 'NONE', 3,
 ( #4196, #10920, #13640, #15221, #1534, #14959, #8545, #11008, #6950, #12509, #8279, #14865, #1442, #394 ),
 .UNSPECIFIED., .F., .F.,
 ( 4, 2, 2, 2, 2, 2, 4 ),
 ( 0.001064030468739382692, 0.001458147099196469747, 0.001852263729653557019, 0.002246380360110644073, 0.002640496990567731128, 0.003428730251481901768, 0.004216963512396073276 ),
 .UNSPECIFIED. ) ;
#15928 = CARTESIAN_POINT ( 'NONE',  ( -3.636496289402155746, 78.53000000000000114, 11.19198476289190936 ) ) ;
#15929 = EDGE_CURVE ( 'NONE', #1713, #368, #9988, .T. ) ;
#15930 = CARTESIAN_POINT ( 'NONE',  ( -17.32050807568884210, 7.773118517290098950, 7.999999999999840128 ) ) ;
#15931 = CARTESIAN_POINT ( 'NONE',  ( 3.989780539755591882, -100.0000000000000568, 13.50333144898421089 ) ) ;
#15932 = CARTESIAN_POINT ( 'NONE',  ( -13.49999999999999822, 34.07999999999999829, 4.386415899144235020 ) ) ;
#15933 = CARTESIAN_POINT ( 'NONE',  ( -8.043339635996302306, -22.89374999999994387, -8.043339635997654113 ) ) ;
#15934 = CARTESIAN_POINT ( 'NONE',  ( 10.99999999999990941, 0.000000000000000000, 15.58845726811995824 ) ) ;
#15935 = CARTESIAN_POINT ( 'NONE',  ( 4.429208140063253474, 34.02068188122268566, -12.75274710002904399 ) ) ;
#15936 = CARTESIAN_POINT ( 'NONE',  ( -7.570064420617500289, 73.46396487899353644, -11.17798062459965358 ) ) ;
#15937 = EDGE_LOOP ( 'NONE', ( #14179, #8691, #1624, #16292 ) ) ;
#15938 = ORIENTED_EDGE ( 'NONE', *, *, #11403, .F. ) ;
#15939 = CARTESIAN_POINT ( 'NONE',  ( -3.636496289402153081, 74.33000000000001251, -11.19198476289190936 ) ) ;
#15940 = ORIENTED_EDGE ( 'NONE', *, *, #848, .T. ) ;
#15941 = CARTESIAN_POINT ( 'NONE',  ( 11.37500000000039613, -74.89062499999985789, -4.711679271993002516 ) ) ;
#15942 = CARTESIAN_POINT ( 'NONE',  ( -7.365732241337891395, 44.40484326663887771, 11.31354391936344506 ) ) ;
#15943 = CARTESIAN_POINT ( 'NONE',  ( 8.351563113033638075, 8.007813505529846054, 16.17460542229567366 ) ) ;
#15944 = CARTESIAN_POINT ( 'NONE',  ( 9.418294590293729840, 66.81060122333079221, -9.677908191170031316 ) ) ;
#15945 = CARTESIAN_POINT ( 'NONE',  ( 8.343458848123578520, 44.97999999999998977, 11.48378591275254124 ) ) ;
#15946 = CARTESIAN_POINT ( 'NONE',  ( -4.476370017849513161, 71.51896129429336213, 12.73625716771306671 ) ) ;
#15947 = ADVANCED_FACE ( 'NONE', ( #2003 ), #6018, .T. ) ;
#15948 = B_SPLINE_CURVE_WITH_KNOTS ( 'NONE', 3,
 ( #11470, #4749, #10155, #2503, #13475, #8198, #13220, #9179, #2414, #14617, #14871, #16202, #17450, #9527, #3938, #3767, #15860, #5283, #14788, #11988, #11903, #13562, #6690, #12072, #1452, #9353, #2678, #3851, #5365, #4113, #1108, #13306, #14528, #7847, #8110, #6524, #5545, #1361, #10667, #17280, #17369, #5194, #6779, #6870 ),
 .UNSPECIFIED., .F., .F.,
 ( 4, 2, 2, 2, 2, 2, 2, 2, 2, 2, 2, 2, 2, 2, 2, 2, 2, 2, 2, 2, 2, 4 ),
 ( 0.03689401835950766734, 0.03766257893388839234, 0.03843113950826912428, 0.03919970008264984929, 0.03996826065703057429, 0.04073682123141130623, 0.04150538180579202430, 0.04304250295455348124, 0.04457962410331493125, 0.04611674525207638820, 0.04765386640083783820, 0.04919098754959928821, 0.05072810869836074515, 0.05226522984712220210, 0.05380235099588365211, 0.05533947214464510905, 0.05687659329340656600, 0.05764515386778729100, 0.05841371444216801601, 0.05995083559092945213, 0.06071939616531016326, 0.06148795673969088826 ),
 .UNSPECIFIED. ) ;
#15949 = AXIS2_PLACEMENT_3D ( 'NONE', #6342, #11728, #3677 ) ;
#15950 = CARTESIAN_POINT ( 'NONE',  ( 13.16986379960055409, 5.168750000000006395, -13.16986379959834430 ) ) ;
#15951 = CARTESIAN_POINT ( 'NONE',  ( -12.89419414780135931, 68.07351481693184780, 3.999877596732322349 ) ) ;
#15952 = CARTESIAN_POINT ( 'NONE',  ( 1.561832610794586538E-12, -87.41249999999979536, -18.62500000000000000 ) ) ;
#15953 = CARTESIAN_POINT ( 'NONE',  ( 3.511521273362200546, 55.05373854301420522, -13.03714384340177368 ) ) ;
#15954 = CARTESIAN_POINT ( 'NONE',  ( -13.16986379959834252, -72.84374999999981526, -13.16986379960055054 ) ) ;
#15955 = CARTESIAN_POINT ( 'NONE',  ( -13.38752141559960762, 64.99072630046104848, 1.739259147947423978 ) ) ;
#15956 = B_SPLINE_CURVE_WITH_KNOTS ( 'NONE', 3,
 ( #10110, #10281, #12657, #2031 ),
 .UNSPECIFIED., .F., .F.,
 ( 4, 4 ),
 ( 0.008786844460939023313, 0.01643317035798798689 ),
 .UNSPECIFIED. ) ;
#15957 = CARTESIAN_POINT ( 'NONE',  ( -2.073600124454130000, 35.60538353478859364, 13.34095837325122069 ) ) ;
#15958 = CARTESIAN_POINT ( 'NONE',  ( -8.343458848123582072, 18.38000000000000611, 11.48378591275254124 ) ) ;
#15959 = ORIENTED_EDGE ( 'NONE', *, *, #7633, .F. ) ;
#15960 = CARTESIAN_POINT ( 'NONE',  ( 10.92172942406179104, 50.72999999999999687, -7.935100905948385908 ) ) ;
#15961 = VECTOR ( 'NONE', #12296, 1000.000000000000000 ) ;
#15962 = CARTESIAN_POINT ( 'NONE',  ( -9.520470885617715595, 27.63000000000001677, -6.917026985038136289 ) ) ;
#15963 = CARTESIAN_POINT ( 'NONE',  ( -4.129380727326757317, 31.32847731590642582, -12.85304772793163863 ) ) ;
#15964 = CYLINDRICAL_SURFACE ( 'NONE', #7974, 13.50000000000000000 ) ;
#15965 = CARTESIAN_POINT ( 'NONE',  ( -9.520470885617715595, -8.369999999999995666, -6.917026985038136289 ) ) ;
#15966 = CARTESIAN_POINT ( 'NONE',  ( 12.86781002116635442, 60.28328535326944149, 4.085762581384763337 ) ) ;
#15967 = CARTESIAN_POINT ( 'NONE',  ( -8.549982208541774191E-16, -5.320000000000001172, 14.19474002721660355 ) ) ;
#15968 = CARTESIAN_POINT ( 'NONE',  ( -11.04090545666283774, 53.22297625534304188, 7.768428304626336711 ) ) ;
#15969 = EDGE_CURVE ( 'NONE', #8605, #13571, #14578, .T. ) ;
#15970 = CARTESIAN_POINT ( 'NONE',  ( 7.272992578804308828, 60.97999999999999687, 10.01041549318726709 ) ) ;
#15971 = CONTEXT_DEPENDENT_SHAPE_REPRESENTATION ( #15320, #1113 ) ;
#15972 = CARTESIAN_POINT ( 'NONE',  ( 8.462697274394789915, 51.00384814321047600, 10.51912736017751904 ) ) ;
#15973 = CARTESIAN_POINT ( 'NONE',  ( -10.98001549286353296, 37.63278772585531584, -7.866452531253198543 ) ) ;
#15974 = CARTESIAN_POINT ( 'NONE',  ( 11.06150406454992030, 36.13825259647077814, 7.739128912404242833 ) ) ;
#15975 = CARTESIAN_POINT ( 'NONE',  ( 8.043339635996298753, -88.41874999999980389, 8.043339635997652337 ) ) ;
#15976 = CARTESIAN_POINT ( 'NONE',  ( -5.241819211398198064, 74.49045729122398996, 12.44079554077151961 ) ) ;
#15977 = CARTESIAN_POINT ( 'NONE',  ( -12.53157464354551287, 76.74754124118879872, -5.020938431400466584 ) ) ;
#15978 = CARTESIAN_POINT ( 'NONE',  ( -12.29521383468573958, 79.72576744650467617, -5.579058808064132791 ) ) ;
#15979 = CARTESIAN_POINT ( 'NONE',  ( 7.272992578804308828, 13.98000000000000220, 10.01041549318726709 ) ) ;
#15980 = CARTESIAN_POINT ( 'NONE',  ( 7.500000000000001776, 108.4800942032927509, 3.560038493048083730 ) ) ;
#15981 = LINE ( 'NONE', #3884, #13140 ) ;
#15982 = CARTESIAN_POINT ( 'NONE',  ( 11.76794919243112680, 2.579999999999996962, -3.823638476888993942 ) ) ;
#15983 = CARTESIAN_POINT ( 'NONE',  ( 7.272992578804308828, 57.97999999999999687, 10.01041549318726886 ) ) ;
#15984 = CARTESIAN_POINT ( 'NONE',  ( 4.711679271993006957, -39.57812499999989342, 11.37500000000039613 ) ) ;
#15985 = CARTESIAN_POINT ( 'NONE',  ( -13.50000000000000000, -4.069999999999997620, -3.469446951953614189E-15 ) ) ;
#15986 = CARTESIAN_POINT ( 'NONE',  ( 6.750022862106053623, 29.92926176209967437, 11.69132975161703669 ) ) ;
#15987 = CARTESIAN_POINT ( 'NONE',  ( 7.265447703103709465, 75.90908602052756748, -11.38066394550858185 ) ) ;
#15988 = CARTESIAN_POINT ( 'NONE',  ( -13.16986379960055231, -93.65624999999977263, 13.16986379959834252 ) ) ;
#15989 = CARTESIAN_POINT ( 'NONE',  ( -9.520470885617717371, 39.23000000000000398, 6.917026985038133624 ) ) ;
#15990 = CARTESIAN_POINT ( 'NONE',  ( 7.500000000000000000, -7.999999999999998224, -22.50000000000000355 ) ) ;
#15991 = CARTESIAN_POINT ( 'NONE',  ( -11.19072645572614100, 58.64612364100203479, -7.551004225710134854 ) ) ;
#15992 = CARTESIAN_POINT ( 'NONE',  ( 2.917162700404270836, 44.78489042209035631, 13.18105316755035439 ) ) ;
#15993 = CARTESIAN_POINT ( 'NONE',  ( 10.15949134898925088, 69.77235859015937081, -8.890162730232345822 ) ) ;
#15994 = CARTESIAN_POINT ( 'NONE',  ( 2.445080149700053643E-15, 54.17999999999999972, -13.50000000000000000 ) ) ;
#15995 = CARTESIAN_POINT ( 'NONE',  ( 9.329993715843995616, 30.04517432730955662, 9.757520963080287046 ) ) ;
#15996 = CARTESIAN_POINT ( 'NONE',  ( -4.170360066879259087, 55.32995151900944819, -12.83978663759837069 ) ) ;
#15997 = CARTESIAN_POINT ( 'NONE',  ( -6.254757922007740945, 50.45086428866937922, 11.96761786975087105 ) ) ;
#15998 = CARTESIAN_POINT ( 'NONE',  ( 9.869871377105818411, 63.78755568821424760, -9.210636547543993302 ) ) ;
#15999 = CARTESIAN_POINT ( 'NONE',  ( 12.13036376994949350, 42.64785262807090049, -5.926645582322720429 ) ) ;
#16000 = CARTESIAN_POINT ( 'NONE',  ( 10.97791377685320668, 39.13320314606657746, 7.859089960518745421 ) ) ;
#16001 = VERTEX_POINT ( 'NONE', #7338 ) ;
#16002 = CARTESIAN_POINT ( 'NONE',  ( -13.20903748930417976, 70.83043373285759969, -2.815464265785562414 ) ) ;
#16003 = LINE ( 'NONE', #12045, #6505 ) ;
#16004 = CARTESIAN_POINT ( 'NONE',  ( -7.272992578804310604, 4.379999999999999005, 10.01041549318726709 ) ) ;
#16005 = ORIENTED_EDGE ( 'NONE', *, *, #9277, .T. ) ;
#16006 = ORIENTED_EDGE ( 'NONE', *, *, #4911, .T. ) ;
#16007 = CARTESIAN_POINT ( 'NONE',  ( 4.171729424061789260, 26.83000000000001961, 12.83926296998457239 ) ) ;
#16008 = CARTESIAN_POINT ( 'NONE',  ( 7.714727599197338748, -80.12812499999981242, 18.62500000000063949 ) ) ;
#16009 = CARTESIAN_POINT ( 'NONE',  ( 3.306959159702415718, 47.79891067118984438, 13.08869937906687397 ) ) ;
#16010 = CARTESIAN_POINT ( 'NONE',  ( 10.92172942406178926, 16.13000000000000611, 7.935100905948385908 ) ) ;
#16011 = CARTESIAN_POINT ( 'NONE',  ( 9.778897066067186117, 72.06775799895999057, 9.307158233501985123 ) ) ;
#16012 = CARTESIAN_POINT ( 'NONE',  ( 12.46723268277846053, 57.24143407219609969, 5.178624223398916371 ) ) ;
#16013 = CARTESIAN_POINT ( 'NONE',  ( -11.76794919243112325, 72.07999999999999829, 3.823638476888994386 ) ) ;
#16014 = CARTESIAN_POINT ( 'NONE',  ( 7.272992578804308828, 78.97999999999998977, 10.01041549318726709 ) ) ;
#16015 = CARTESIAN_POINT ( 'NONE',  ( -3.824707916743821379, 47.54247761955691942, 12.94687856268078896 ) ) ;
#16016 = CARTESIAN_POINT ( 'NONE',  ( 18.71141623506677121, 7.854708462831346161, 1.539237008743780555 ) ) ;
#16017 = CARTESIAN_POINT ( 'NONE',  ( 7.585183428008853923, -99.99999999999978684, 15.21066662881120202 ) ) ;
#16018 = DIRECTION ( 'NONE',  ( 0.000000000000000000, 0.000000000000000000, -1.000000000000000000 ) ) ;
#16019 = CARTESIAN_POINT ( 'NONE',  ( -4.711679271993004292, -38.50312499999991189, -11.37500000000039435 ) ) ;
#16020 = LINE ( 'NONE', #14517, #16266 ) ;
#16021 = CARTESIAN_POINT ( 'NONE',  ( 11.26022822739175844, 33.70954470917394730, -7.446967326473597382 ) ) ;
#16022 = CARTESIAN_POINT ( 'NONE',  ( -2.238595305369822430, 73.26049135710265148, -13.31312577019137322 ) ) ;
#16023 = ORIENTED_EDGE ( 'NONE', *, *, #9474, .T. ) ;
#16024 = EDGE_CURVE ( 'NONE', #11876, #9086, #12784, .T. ) ;
#16025 = ORIENTED_EDGE ( 'NONE', *, *, #17286, .T. ) ;
#16026 = CARTESIAN_POINT ( 'NONE',  ( 11.76794919243112325, 73.27999999999998693, 3.823638476888997051 ) ) ;
#16027 = VERTEX_POINT ( 'NONE', #12809 ) ;
#16028 = CARTESIAN_POINT ( 'NONE',  ( 2.279995255611139653E-15, -11.81999999999999851, -12.37355403259654985 ) ) ;
#16029 = CARTESIAN_POINT ( 'NONE',  ( -11.37499999999999645, -98.82499999999978968, -9.545674412382054647E-13 ) ) ;
#16030 = CARTESIAN_POINT ( 'NONE',  ( 10.18318151426813323, 7.956016702382084915, 15.32135601632713673 ) ) ;
#16031 = VECTOR ( 'NONE', #10822, 1000.000000000000000 ) ;
#16032 = CARTESIAN_POINT ( 'NONE',  ( 13.50000000000000000, 45.42999999999999972, 1.653273178848926867E-15 ) ) ;
#16033 = CARTESIAN_POINT ( 'NONE',  ( -5.757915664079544804, 71.47057076169542711, 12.21051929849135220 ) ) ;
#16034 = CARTESIAN_POINT ( 'NONE',  ( -1.564113515457998370E-12, -5.237499999999969624, 18.62500000000000000 ) ) ;
#16035 = CARTESIAN_POINT ( 'NONE',  ( -13.42122754482370262, 67.98067473477300382, 1.456274877649156085 ) ) ;
#16036 = CARTESIAN_POINT ( 'NONE',  ( -7.714727599200467800, -78.04687499999982947, 18.62499999999934630 ) ) ;
#16037 = CARTESIAN_POINT ( 'NONE',  ( 6.362841488961052505, 54.94654819462200379, -11.90648129171133540 ) ) ;
#16038 = VECTOR ( 'NONE', #6013, 1000.000000000000000 ) ;
#16039 = CARTESIAN_POINT ( 'NONE',  ( 11.76794919243112680, 17.57999999999999829, -3.823638476888993942 ) ) ;
#16040 = CARTESIAN_POINT ( 'NONE',  ( -13.16986379959834252, -89.49374999999979252, -13.16986379960055054 ) ) ;
#16041 = CARTESIAN_POINT ( 'NONE',  ( -13.43293025143715980, 64.88277759376563836, -1.363649920549056427 ) ) ;
#16042 = EDGE_CURVE ( 'NONE', #9933, #4018, #3431, .T. ) ;
#16043 = CARTESIAN_POINT ( 'NONE',  ( -5.833452229489934915, 35.46778541590376221, 12.18399501181652234 ) ) ;
#16044 = ORIENTED_EDGE ( 'NONE', *, *, #16745, .T. ) ;
#16045 = DIRECTION ( 'NONE',  ( -0.000000000000000000, 1.000000000000000000, -0.000000000000000000 ) ) ;
#16046 = CARTESIAN_POINT ( 'NONE',  ( -5.441113646577659502, 0.000000000000000000, 25.42428528562849976 ) ) ;
#16047 = CARTESIAN_POINT ( 'NONE',  ( -10.03785665333376009, 31.58129449068416150, -9.027804630255781504 ) ) ;
#16048 = LINE ( 'NONE', #6624, #5146 ) ;
#16049 = CARTESIAN_POINT ( 'NONE',  ( -11.76794919243112325, -10.92000000000000526, 3.823638476888994386 ) ) ;
#16050 = CARTESIAN_POINT ( 'NONE',  ( 1.279986136922147688, 59.72594881717020598, 13.44789384724496273 ) ) ;
#16051 = CARTESIAN_POINT ( 'NONE',  ( -8.343458848123576743, -9.520000000000006679, -11.48378591275254301 ) ) ;
#16052 = CARTESIAN_POINT ( 'NONE',  ( -11.19291883443861657, 53.21376446446998898, 7.548464480317238490 ) ) ;
#16053 = CIRCLE ( 'NONE', #10163, 14.50000000000000000 ) ;
#16054 = CARTESIAN_POINT ( 'NONE',  ( -3.636496289402153081, 50.32999999999999829, -11.19198476289190936 ) ) ;
#16055 = DIRECTION ( 'NONE',  ( 1.000000000000000000, 0.000000000000000000, 0.000000000000000000 ) ) ;
#16056 = CARTESIAN_POINT ( 'NONE',  ( -8.343458848123576743, 66.48000000000000398, -11.48378591275254301 ) ) ;
#16057 = CARTESIAN_POINT ( 'NONE',  ( 10.67457095955382940, 51.11584628598345148, 8.264605577784157830 ) ) ;
#16058 = CARTESIAN_POINT ( 'NONE',  ( -10.23347952021401674, 37.59159613339581085, -8.804879535122106304 ) ) ;
#16059 = CARTESIAN_POINT ( 'NONE',  ( 11.11366064790290942, 36.14140235628833864, 7.664027378569688409 ) ) ;
#16060 = CARTESIAN_POINT ( 'NONE',  ( 18.62499999999935341, -22.85937499999996803, 7.714727599200469577 ) ) ;
#16061 = CARTESIAN_POINT ( 'NONE',  ( -0.6302266402344979257, 74.65733938539632675, 13.48528206095811832 ) ) ;
#16062 = CARTESIAN_POINT ( 'NONE',  ( -13.45527179458574807, 76.88938923464503716, -1.166449261855087238 ) ) ;
#16063 = ADVANCED_FACE ( 'NONE', ( #1918 ), #12549, .T. ) ;
#16064 = CARTESIAN_POINT ( 'NONE',  ( -10.96774680160861415, 80.22729587279039265, 7.871546463532750337 ) ) ;
#16065 = CARTESIAN_POINT ( 'NONE',  ( -9.520470885617715595, 9.629999999999999005, -6.917026985038136289 ) ) ;
#16066 = CARTESIAN_POINT ( 'NONE',  ( 7.500000000000000888, 103.9506177843311860, 9.262340467025643065 ) ) ;
#16067 = DIRECTION ( 'NONE',  ( -0.000000000000000000, -1.000000000000000000, -0.000000000000000000 ) ) ;
#16068 = CARTESIAN_POINT ( 'NONE',  ( -11.76794919243112325, 0.9300000000000141487, -2.602085213965210642E-15 ) ) ;
#16069 = CARTESIAN_POINT ( 'NONE',  ( 3.636496289402157078, 47.02999999999999403, -11.19198476289190936 ) ) ;
#16070 = CARTESIAN_POINT ( 'NONE',  ( 8.043339635997652337, -61.43124999999983515, -8.043339635996304082 ) ) ;
#16071 = CARTESIAN_POINT ( 'NONE',  ( -18.62500000000000000, -24.97499999999994102, -1.562973063126292555E-12 ) ) ;
#16072 = CARTESIAN_POINT ( 'NONE',  ( 13.50000000000000355, -5.419999999999997264, -4.386415899144233244 ) ) ;
#16073 = CARTESIAN_POINT ( 'NONE',  ( 5.155428299699167383, 75.99355700656670365, -12.48322344288936314 ) ) ;
#16074 = CARTESIAN_POINT ( 'NONE',  ( 4.178864255851000829E-14, 67.68000000000000682, 13.50000000000000000 ) ) ;
#16075 = CARTESIAN_POINT ( 'NONE',  ( -11.76794919243112325, 35.77999999999999403, -3.823638476888998827 ) ) ;
#16076 = CARTESIAN_POINT ( 'NONE',  ( -1.134839703165779312, 41.63935813733207425, 13.50000000016827606 ) ) ;
#16077 = CARTESIAN_POINT ( 'NONE',  ( -8.937188087482237364, 58.52611931063565009, -10.11856336318372307 ) ) ;
#16078 = FACE_OUTER_BOUND ( 'NONE', #395, .T. ) ;
#16079 = LINE ( 'NONE', #13436, #15961 ) ;
#16080 = DIRECTION ( 'NONE',  ( 0.000000000000000000, 1.000000000000000000, 0.000000000000000000 ) ) ;
#16081 = CARTESIAN_POINT ( 'NONE',  ( -11.20803178499709851, 55.64719445998460401, -7.525311190684723428 ) ) ;
#16082 = CARTESIAN_POINT ( 'NONE',  ( -13.30613126912205679, 49.84985106113156661, -2.280881810908200080 ) ) ;
#16083 = CARTESIAN_POINT ( 'NONE',  ( 12.45879162498721904, 63.61962684891894781, -5.206934220104953326 ) ) ;
#16084 = CARTESIAN_POINT ( 'NONE',  ( 11.08960580799031170, 42.72000896289767269, -7.699079133861338242 ) ) ;
#16085 = CARTESIAN_POINT ( 'NONE',  ( 10.86487605210494145, 39.12658062121423086, 8.013745105519641143 ) ) ;
#16086 = ORIENTED_EDGE ( 'NONE', *, *, #4815, .F. ) ;
#16087 = CARTESIAN_POINT ( 'NONE',  ( -12.80368829784359974, 70.77590667484511755, -4.279836677223643804 ) ) ;
#16088 = CARTESIAN_POINT ( 'NONE',  ( -8.343458848123582072, 49.37999999999999545, 11.48378591275253768 ) ) ;
#16089 = ORIENTED_EDGE ( 'NONE', *, *, #16937, .F. ) ;
#16090 = VERTEX_POINT ( 'NONE', #14030 ) ;
#16091 = CARTESIAN_POINT ( 'NONE',  ( -10.92172942406178926, 25.63000000000001322, -7.935100905948389460 ) ) ;
#16092 = CARTESIAN_POINT ( 'NONE',  ( 1.561832610794586538E-12, -87.41249999999979536, -18.62500000000000000 ) ) ;
#16093 = CARTESIAN_POINT ( 'NONE',  ( 4.869579850628348971, 61.00451404086120988, -12.59138024303687509 ) ) ;
#16094 = CARTESIAN_POINT ( 'NONE',  ( -8.343458848123582072, 12.37999999999999368, 11.48378591275254124 ) ) ;
#16095 = CARTESIAN_POINT ( 'NONE',  ( 0.000000000000000000, 9.000000000000000000, 0.000000000000000000 ) ) ;
#16096 = CARTESIAN_POINT ( 'NONE',  ( 12.00451621900212729, 57.65805921716241045, -6.182138200911872161 ) ) ;
#16097 = CARTESIAN_POINT ( 'NONE',  ( 9.520470885617717371, 64.72999999999998977, -6.917026985038131848 ) ) ;
#16098 = CARTESIAN_POINT ( 'NONE',  ( -7.576616670048093940E-16, 78.67999999999999261, 12.37355403259654985 ) ) ;
#16099 = CARTESIAN_POINT ( 'NONE',  ( -7.090376077374727082, 47.41654259168927155, 11.48810848389221739 ) ) ;
#16100 = EDGE_CURVE ( 'NONE', #8734, #11528, #1595, .T. ) ;
#16101 = CARTESIAN_POINT ( 'NONE',  ( 1.876532330890708260E-11, 6.313974596214807278, -12.00000000000000355 ) ) ;
#16102 = CARTESIAN_POINT ( 'NONE',  ( 18.28286893203052799, -100.0000000000000142, 3.421288217922580976 ) ) ;
#16103 = DIRECTION ( 'NONE',  ( -0.000000000000000000, 1.000000000000000000, -0.000000000000000000 ) ) ;
#16104 = CARTESIAN_POINT ( 'NONE',  ( -11.37499999999960387, -23.93437499999993889, -4.711679271994910323 ) ) ;
#16105 = CARTESIAN_POINT ( 'NONE',  ( -8.343458848123578520, 39.48000000000000398, -11.48378591275254124 ) ) ;
#16106 = CARTESIAN_POINT ( 'NONE',  ( 12.13600343332003817, 33.64737785006074233, -5.914467048366985225 ) ) ;
#16107 = CARTESIAN_POINT ( 'NONE',  ( -9.603217289138866519, 73.55881626489666303, -9.488364816495691301 ) ) ;
#16108 = ORIENTED_EDGE ( 'NONE', *, *, #13247, .F. ) ;
#16109 = VERTEX_POINT ( 'NONE', #15005 ) ;
#16110 = CARTESIAN_POINT ( 'NONE',  ( 9.520470885617715595, 79.13000000000000966, 6.917026985038134512 ) ) ;
#16111 = ORIENTED_EDGE ( 'NONE', *, *, #13461, .T. ) ;
#16112 = CARTESIAN_POINT ( 'NONE',  ( -18.62499999999935341, -14.53437499999998650, -7.714727599200458030 ) ) ;
#16113 = CARTESIAN_POINT ( 'NONE',  ( -4.963731793517477620, 44.50093815360280303, 12.55597456324973216 ) ) ;
#16114 = DIRECTION ( 'NONE',  ( 1.000000000000000000, 0.000000000000000000, 0.000000000000000000 ) ) ;
#16115 = CARTESIAN_POINT ( 'NONE',  ( -13.50000000000000000, 46.92999999999999972, -3.306546357697853733E-15 ) ) ;
#16116 = CARTESIAN_POINT ( 'NONE',  ( -13.45369161577737849, 70.89049427693734629, -1.140183565930726228 ) ) ;
#16117 = EDGE_CURVE ( 'NONE', #12212, #1976, #16734, .T. ) ;
#16118 = CARTESIAN_POINT ( 'NONE',  ( 13.16986379959833897, -23.96874999999992539, 13.16986379960055409 ) ) ;
#16119 = CARTESIAN_POINT ( 'NONE',  ( -13.38782401986913051, 67.99071915777986419, 1.738903060278587320 ) ) ;
#16120 = CARTESIAN_POINT ( 'NONE',  ( -1.564113515457998572E-12, -95.73749999999976978, 18.62500000000000000 ) ) ;
#16121 = AXIS2_PLACEMENT_3D ( 'NONE', #12377, #8243, #2898 ) ;
#16122 = CARTESIAN_POINT ( 'NONE',  ( 13.01113393269324092, 54.30141377912826783, 3.601429272714332441 ) ) ;
#16123 = CARTESIAN_POINT ( 'NONE',  ( -18.62500000000000000, -91.57499999999977547, -1.562973063126292555E-12 ) ) ;
#16124 = CARTESIAN_POINT ( 'NONE',  ( -12.53153993143703460, 64.74693242360650913, -5.040447919499604801 ) ) ;
#16125 = CARTESIAN_POINT ( 'NONE',  ( -12.24515502415462365, 35.13909831631156777, 5.707366899919843917 ) ) ;
#16126 = ORIENTED_EDGE ( 'NONE', *, *, #986, .F. ) ;
#16127 = CARTESIAN_POINT ( 'NONE',  ( -6.381610013855579133, 2.177477983142718114E-15, -10.81467641374194422 ) ) ;
#16128 = CARTESIAN_POINT ( 'NONE',  ( -11.34467727478165777, 31.65563633594693016, -7.320944989841013495 ) ) ;
#16129 = CARTESIAN_POINT ( 'NONE',  ( 4.953012991158001199, 73.00140879485633150, -12.55898227005201662 ) ) ;
#16130 = CARTESIAN_POINT ( 'NONE',  ( -9.520470885617717371, -10.76999999999999424, 6.917026985038133624 ) ) ;
#16131 = DIRECTION ( 'NONE',  ( 9.637352644315600173E-17, -1.000000000000000000, 0.000000000000000000 ) ) ;
#16132 = CARTESIAN_POINT ( 'NONE',  ( -10.92172942406178926, -6.370000000000000995, -7.935100905948389460 ) ) ;
#16133 = CARTESIAN_POINT ( 'NONE',  ( -12.91130779797210337, 52.78849919330026097, -3.946434418955392598 ) ) ;
#16134 = CIRCLE ( 'NONE', #13054, 26.00000000000000355 ) ;
#16135 = CARTESIAN_POINT ( 'NONE',  ( -7.272992578804310604, 45.38000000000000256, 10.01041549318726709 ) ) ;
#16136 = SHAPE_DEFINITION_REPRESENTATION ( #3797, #8052 ) ;
#16137 = CARTESIAN_POINT ( 'NONE',  ( -8.343458848123576743, 69.47999999999998977, -11.48378591275254301 ) ) ;
#16138 = ADVANCED_FACE ( 'NONE', ( #8328, #6646 ), #6999, .F. ) ;
#16139 = CARTESIAN_POINT ( 'NONE',  ( 7.795000087196527261, 50.97370711654939157, 11.02690683953273876 ) ) ;
#16140 = CARTESIAN_POINT ( 'NONE',  ( -10.29227820885054712, 37.59468482203347861, -8.736150211427487378 ) ) ;
#16141 = CARTESIAN_POINT ( 'NONE',  ( 4.962760302008886626, 35.85893607516423742, 12.55665820087269680 ) ) ;
#16142 = CARTESIAN_POINT ( 'NONE',  ( 18.62500000000000000, -7.250000000000001776, 1.560692158462880521E-12 ) ) ;
#16143 = CARTESIAN_POINT ( 'NONE',  ( -12.04168536818074209, 74.15490546771334834, 6.103169336798146993 ) ) ;
#16144 = CARTESIAN_POINT ( 'NONE',  ( -12.58168582133113844, 76.75239693361646687, -4.895191552310046212 ) ) ;
#16145 = VECTOR ( 'NONE', #8142, 1000.000000000000000 ) ;
#16146 = CARTESIAN_POINT ( 'NONE',  ( -7.311972143045258221, 80.40722760048129203, 11.35053210907591570 ) ) ;
#16147 = CARTESIAN_POINT ( 'NONE',  ( -9.520470885617717371, 10.23000000000000220, 6.917026985038133624 ) ) ;
#16148 = DIRECTION ( 'NONE',  ( 0.000000000000000000, 0.000000000000000000, 1.000000000000000000 ) ) ;
#16149 = CARTESIAN_POINT ( 'NONE',  ( -2.138189944381240881, 8.603118577679731871, 13.49999999999999822 ) ) ;
#16150 = CARTESIAN_POINT ( 'NONE',  ( 2.279995255611139653E-15, 3.180000000000006821, -12.37355403259654985 ) ) ;
#16151 = CARTESIAN_POINT ( 'NONE',  ( -11.76794919243112325, 50.77999999999999403, -3.823638476888998827 ) ) ;
#16152 = CARTESIAN_POINT ( 'NONE',  ( 9.538709233711902776E-13, -37.46249999999991331, -11.37500000000000000 ) ) ;
#16153 = CARTESIAN_POINT ( 'NONE',  ( 1.561832610794586538E-12, -37.46249999999991331, -18.62500000000000000 ) ) ;
#16154 = CARTESIAN_POINT ( 'NONE',  ( 4.171729424061789260, -12.16999999999999993, 12.83926296998457239 ) ) ;
#16155 = CARTESIAN_POINT ( 'NONE',  ( -10.26574468177152433, 40.59333272807688076, -8.767239472786558352 ) ) ;
#16156 = FACE_BOUND ( 'NONE', #9960, .T. ) ;
#16157 = CARTESIAN_POINT ( 'NONE',  ( 10.60663207285976029, 75.11149614483424841, 8.363159649599104739 ) ) ;
#16158 = CARTESIAN_POINT ( 'NONE',  ( 8.343458848123583849, 68.87999999999999545, -11.48378591275253768 ) ) ;
#16159 = CARTESIAN_POINT ( 'NONE',  ( -7.576616670048093940E-16, 42.67999999999999972, 12.37355403259654985 ) ) ;
#16160 = CARTESIAN_POINT ( 'NONE',  ( -9.179761508417909610, 41.32223751179169113, 9.899410405694473170 ) ) ;
#16161 = CARTESIAN_POINT ( 'NONE',  ( -5.154035034630091161, 58.36612174761953753, -12.48310025089808661 ) ) ;
#16162 = DIRECTION ( 'NONE',  ( 0.000000000000000000, 0.000000000000000000, 1.000000000000000000 ) ) ;
#16163 = CARTESIAN_POINT ( 'NONE',  ( 0.000000000000000000, 0.000000000000000000, 0.000000000000000000 ) ) ;
#16164 = CARTESIAN_POINT ( 'NONE',  ( -1.900613283894433403, 3.390856018535834515, -12.00000000000000355 ) ) ;
#16165 = PLANE ( 'NONE',  #1194 ) ;
#16166 = CARTESIAN_POINT ( 'NONE',  ( -7.404372219800137600, 49.45681430499143261, -11.28829308273742527 ) ) ;
#16167 = CARTESIAN_POINT ( 'NONE',  ( 13.47648628015202910, 63.46132184567057521, -0.9086240695849856497 ) ) ;
#16168 = CARTESIAN_POINT ( 'NONE',  ( 10.75640908300814047, 42.73960387034645692, -8.162873688883740542 ) ) ;
#16170 = CARTESIAN_POINT ( 'NONE',  ( -18.02388005911709712, 8.055054232036098938, 0.3546005442043826394 ) ) ;
#16169 = B_SPLINE_CURVE_WITH_KNOTS ( 'NONE', 3,
 ( #5669, #8409, #12547, #13761 ),
 .UNSPECIFIED., .F., .F.,
 ( 4, 4 ),
 ( 0.008786844460939023313, 0.01643317035798799036 ),
 .UNSPECIFIED. ) ;
#16171 = VERTEX_POINT ( 'NONE', #13344 ) ;
#16172 = CARTESIAN_POINT ( 'NONE',  ( 0.000000000000000000, 5.918584287042170544, 0.000000000000000000 ) ) ;
#16173 = CARTESIAN_POINT ( 'NONE',  ( 8.043339635997654113, -2.081249999999994493, -8.043339635996304082 ) ) ;
#16174 = ORIENTED_EDGE ( 'NONE', *, *, #15340, .T. ) ;
#16175 = CARTESIAN_POINT ( 'NONE',  ( -5.638841895279958827, 43.38479360352132375, -12.26596786634416247 ) ) ;
#16176 = CARTESIAN_POINT ( 'NONE',  ( -18.62500000000064659, -92.61562499999978115, 7.714727599197335195 ) ) ;
#16177 = CARTESIAN_POINT ( 'NONE',  ( 12.95177247807359677, 60.56636384927607253, -3.809567037313156934 ) ) ;
#16178 = CARTESIAN_POINT ( 'NONE',  ( 8.343458848123578520, 15.97999999999999332, 11.48378591275254124 ) ) ;
#16179 = CARTESIAN_POINT ( 'NONE',  ( 3.375869881531517347, 71.80049840645031622, 13.10095937201164773 ) ) ;
#16180 = CARTESIAN_POINT ( 'NONE',  ( 13.49835085908630461, 57.43768004746023337, -0.2240883959220789090 ) ) ;
#16181 = CARTESIAN_POINT ( 'NONE',  ( -11.76794919243112325, 71.78000000000000114, -3.823638476888998827 ) ) ;
#16182 = CARTESIAN_POINT ( 'NONE',  ( -11.76794919243112325, 77.92999999999999261, -2.882316262207890869E-15 ) ) ;
#16183 = CARTESIAN_POINT ( 'NONE',  ( -3.838951629330794368, 47.54196545468892054, 12.94266222818414391 ) ) ;
#16184 = DIRECTION ( 'NONE',  ( 0.000000000000000000, -1.000000000000000000, 0.000000000000000000 ) ) ;
#16185 = CARTESIAN_POINT ( 'NONE',  ( 0.000000000000000000, 80.93000000000000682, 0.000000000000000000 ) ) ;
#16186 = CARTESIAN_POINT ( 'NONE',  ( 4.171729424061789260, 37.82999999999999829, 12.83926296998457417 ) ) ;
#16187 = CARTESIAN_POINT ( 'NONE',  ( -8.343458848123582072, 34.37999999999999545, 11.48378591275253768 ) ) ;
#16188 = CARTESIAN_POINT ( 'NONE',  ( 8.043339635997654113, -2.081249999999994493, -8.043339635996304082 ) ) ;
#16189 = CARTESIAN_POINT ( 'NONE',  ( -13.49999999999999822, 51.78000000000000114, -4.386415899144240349 ) ) ;
#16190 = CARTESIAN_POINT ( 'NONE',  ( 11.25128164550088528, 33.71009814866270915, -7.460485725860525719 ) ) ;
#16191 = CARTESIAN_POINT ( 'NONE',  ( -3.559128983600132745, 73.30801538557933839, -13.02258798672816553 ) ) ;
#16192 = CARTESIAN_POINT ( 'NONE',  ( 5.578754407927415393, 39.97753789112579881, -12.30135392881136625 ) ) ;
#16193 = ORIENTED_EDGE ( 'NONE', *, *, #5033, .T. ) ;
#16194 = CARTESIAN_POINT ( 'NONE',  ( -9.520470885617717371, 25.23000000000000398, 6.917026985038133624 ) ) ;
#16195 = CARTESIAN_POINT ( 'NONE',  ( -4.310519988233258992, 62.52494779739406283, 12.79455156266785743 ) ) ;
#16196 = ORIENTED_EDGE ( 'NONE', *, *, #14875, .F. ) ;
#16197 = CARTESIAN_POINT ( 'NONE',  ( -13.48481038722050762, 40.90780079122387747, -0.6425594624344264094 ) ) ;
#16198 = CARTESIAN_POINT ( 'NONE',  ( 11.76794919243112325, -12.56999999999999851, 1.734723475976807094E-15 ) ) ;
#16199 = CARTESIAN_POINT ( 'NONE',  ( -8.043339635997652337, -84.25624999999980957, 8.043339635996300530 ) ) ;
#16200 = EDGE_CURVE ( 'NONE', #7799, #6926, #8633, .T. ) ;
#16201 = CARTESIAN_POINT ( 'NONE',  ( -10.54105442489647970, 44.25196237461326376, 8.439972557216172788 ) ) ;
#16202 = CARTESIAN_POINT ( 'NONE',  ( -7.499999999999994671, -25.65063367634388314, -7.726132535793207801 ) ) ;
#16203 = CARTESIAN_POINT ( 'NONE',  ( 8.343458848123583849, 42.87999999999998124, -11.48378591275253768 ) ) ;
#16204 = CARTESIAN_POINT ( 'NONE',  ( -10.92172942406178926, 45.62999999999999545, -7.935100905948389460 ) ) ;
#16205 = CARTESIAN_POINT ( 'NONE',  ( -12.39285729354113386, 71.12555814250139008, 5.359515616412462435 ) ) ;
#16206 = PRODUCT ( 'Top rod', 'Top rod', '', ( #4047 ) ) ;
#16207 = CARTESIAN_POINT ( 'NONE',  ( 18.62500000000000000, -59.34999999999983800, 1.560692158462880521E-12 ) ) ;
#16208 = CARTESIAN_POINT ( 'NONE',  ( -11.66385489473767301, 68.18283448863054730, 6.797391872370236676 ) ) ;
#16209 = CARTESIAN_POINT ( 'NONE',  ( -18.62500000000000000, -34.37499999999990052, -1.562973063126292757E-12 ) ) ;
#16210 = CARTESIAN_POINT ( 'NONE',  ( 13.24525085617974440, 54.52251518681887887, -2.621468703140126699 ) ) ;
#16211 = CARTESIAN_POINT ( 'NONE',  ( -18.62499999999934985, -90.53437499999978400, -7.714727599200458918 ) ) ;
#16212 = CARTESIAN_POINT ( 'NONE',  ( -13.50064150216613967, 64.92368711864446595, -0.1755260359765862255 ) ) ;
#16213 = ORIENTED_EDGE ( 'NONE', *, *, #3133, .F. ) ;
#16214 = CARTESIAN_POINT ( 'NONE',  ( -10.92172942406179104, 64.23000000000000398, 7.935100905948387684 ) ) ;
#16215 = CARTESIAN_POINT ( 'NONE',  ( -13.41438580105313250, 34.98340168545936280, 1.533709452862849432 ) ) ;
#16216 = VERTEX_POINT ( 'NONE', #6731 ) ;
#16217 = CARTESIAN_POINT ( 'NONE',  ( -12.24945618364706057, -1.497824325258500411E-15, -4.612754215402016023 ) ) ;
#16218 = CARTESIAN_POINT ( 'NONE',  ( 0.000000000000000000, 3.000000000000000000, -22.50000000000000355 ) ) ;
#16219 = CARTESIAN_POINT ( 'NONE',  ( 6.048413154619182386, 72.95913537431300711, -12.06944015503662015 ) ) ;
#16220 = CARTESIAN_POINT ( 'NONE',  ( -7.272992578804307939, -8.520000000000001350, -10.01041549318726886 ) ) ;
#16221 = CARTESIAN_POINT ( 'NONE',  ( 0.01655142509043793300, 79.17940487182032427, -13.50000000189450944 ) ) ;
#16222 = CARTESIAN_POINT ( 'NONE',  ( 4.171729424061789260, -17.16999999999999815, 12.83926296998457239 ) ) ;
#16223 = VECTOR ( 'NONE', #8143, 1000.000000000000000 ) ;
#16224 = CARTESIAN_POINT ( 'NONE',  ( -8.343458848123582072, 71.37999999999998124, 11.48378591275254124 ) ) ;
#16225 = CARTESIAN_POINT ( 'NONE',  ( -12.46884852525094267, 52.74141282856401602, -5.180859845137886666 ) ) ;
#16226 = APPLICATION_CONTEXT ( 'automotive_design' ) ;
#16227 = CARTESIAN_POINT ( 'NONE',  ( 3.636496289402157078, 50.03000000000000114, -11.19198476289190936 ) ) ;
#16228 = CARTESIAN_POINT ( 'NONE',  ( 4.171729424061791924, 69.03000000000000114, -12.83926296998457239 ) ) ;
#16229 = CARTESIAN_POINT ( 'NONE',  ( 3.035063162148505356, 50.78921730790684563, 13.15580992881729294 ) ) ;
#16230 = CARTESIAN_POINT ( 'NONE',  ( -10.35412786390899242, 37.59795970053211533, -8.662983390277185336 ) ) ;
#16231 = CARTESIAN_POINT ( 'NONE',  ( 12.13297431269409721, 36.20992223033864832, 5.984304902545243721 ) ) ;
#16232 = CARTESIAN_POINT ( 'NONE',  ( 1.561832610794586740E-12, -28.06249999999995381, -18.62500000000000000 ) ) ;
#16233 = CARTESIAN_POINT ( 'NONE',  ( -9.166717776978838828, 74.32310361984721681, 9.924026101965260693 ) ) ;
#16234 = AXIS2_PLACEMENT_3D ( 'NONE', #9815, #9942, #3192 ) ;
#16235 = CARTESIAN_POINT ( 'NONE',  ( -12.49080795396548815, 76.74364347244760154, -5.121680526097208919 ) ) ;
#16236 = CARTESIAN_POINT ( 'NONE',  ( -10.90667313324132159, 80.23087602101854543, 7.955953418439746017 ) ) ;
#16237 = CARTESIAN_POINT ( 'NONE',  ( 2.222800136090958073E-15, 0.04602540378443767399, -12.00000000000000000 ) ) ;
#16238 = CARTESIAN_POINT ( 'NONE',  ( 6.767892274421971166, 80.93000000000000682, 11.68099457074693603 ) ) ;
#16239 = DIRECTION ( 'NONE',  ( -0.000000000000000000, -1.000000000000000000, -0.000000000000000000 ) ) ;
#16240 = CARTESIAN_POINT ( 'NONE',  ( -11.76794919243112325, 1.080000000000000959, 3.823638476888994386 ) ) ;
#16241 = EDGE_CURVE ( 'NONE', #201, #13302, #16454, .T. ) ;
#16242 = CARTESIAN_POINT ( 'NONE',  ( 7.272992578804311492, 43.87999999999999545, -10.01041549318726886 ) ) ;
#16243 = CARTESIAN_POINT ( 'NONE',  ( 4.711679271994909435, -36.42187499999990763, -11.37499999999960387 ) ) ;
#16244 = CARTESIAN_POINT ( 'NONE',  ( -1.328658795546723038E-07, 9.679996299052479714, 13.49999999999999822 ) ) ;
#16245 = CARTESIAN_POINT ( 'NONE',  ( -10.92172942406178926, -10.36999999999999744, -7.935100905948389460 ) ) ;
#16246 = EDGE_CURVE ( 'NONE', #10491, #17339, #2444, .T. ) ;
#16247 = CARTESIAN_POINT ( 'NONE',  ( -10.26587049905779203, 40.59333933079368251, -8.767092715570713679 ) ) ;
#16248 = DIRECTION ( 'NONE',  ( -0.000000000000000000, -1.000000000000000000, -0.000000000000000000 ) ) ;
#16249 = CARTESIAN_POINT ( 'NONE',  ( 10.21052318205141596, 75.09041434710640317, 8.831544897976421282 ) ) ;
#16250 = CARTESIAN_POINT ( 'NONE',  ( 5.127128379249549894, -7.251940901129065153E-16, -15.62300691738110636 ) ) ;
#16251 = VECTOR ( 'NONE', #7985, 1000.000000000000000 ) ;
#16252 = CARTESIAN_POINT ( 'NONE',  ( 11.76794919243112680, 31.57999999999999119, -3.823638476888993942 ) ) ;
#16253 = CARTESIAN_POINT ( 'NONE',  ( -10.44494405107816171, 41.25745373380726022, 8.565014912321151641 ) ) ;
#16254 = CARTESIAN_POINT ( 'NONE',  ( -4.116521602011985692, 58.32801495984301710, -12.85716709580777106 ) ) ;
#16255 = CARTESIAN_POINT ( 'NONE',  ( 4.599859061830847473, 44.84556242937287607, 12.69217623624271241 ) ) ;
#16256 = DIRECTION ( 'NONE',  ( 0.000000000000000000, 0.000000000000000000, 1.000000000000000000 ) ) ;
#16257 = CARTESIAN_POINT ( 'NONE',  ( 9.067440962954476547, 30.03237675404078288, 10.00200502765567556 ) ) ;
#16258 = CARTESIAN_POINT ( 'NONE',  ( -0.4341634609568034708, 55.19561065720218096, -13.49312043558511220 ) ) ;
#16259 = CARTESIAN_POINT ( 'NONE',  ( -10.28297219357257575, 49.59413489483298321, -8.747922443422563532 ) ) ;
#16260 = CARTESIAN_POINT ( 'NONE',  ( 12.79341215383903041, 63.58529488098010773, -4.311560995242466277 ) ) ;
#16261 = CARTESIAN_POINT ( 'NONE',  ( 10.67220332885768030, 42.11571253605529108, 8.267673668127477171 ) ) ;
#16262 = CARTESIAN_POINT ( 'NONE',  ( 6.553170660267079839, 38.92104680671067740, 11.80483472479301099 ) ) ;
#16263 = ORIENTED_EDGE ( 'NONE', *, *, #10680, .F. ) ;
#16264 = CARTESIAN_POINT ( 'NONE',  ( -2.610032936771094825, 70.27384716112842966, -13.24532283237781627 ) ) ;
#16265 = CARTESIAN_POINT ( 'NONE',  ( -10.92172942406178926, 48.63000000000000256, -7.935100905948389460 ) ) ;
#16266 = VECTOR ( 'NONE', #3927, 1000.000000000000000 ) ;
#16267 = CARTESIAN_POINT ( 'NONE',  ( -8.343458848123582072, 11.38000000000001144, 11.48378591275254124 ) ) ;
#16268 = ORIENTED_EDGE ( 'NONE', *, *, #5823, .F. ) ;
#16269 = EDGE_CURVE ( 'NONE', #4638, #9259, #10620, .T. ) ;
#16270 = CARTESIAN_POINT ( 'NONE',  ( -8.491832788201611137, 43.50521800093334690, -10.49509145101893459 ) ) ;
#16271 = CARTESIAN_POINT ( 'NONE',  ( -7.499999999999999112, 106.7516370761002520, 7.534909587719529789 ) ) ;
#16272 = CARTESIAN_POINT ( 'NONE',  ( 10.60253966551696614, 60.74819985123946964, -8.356982296996902093 ) ) ;
#16273 = CARTESIAN_POINT ( 'NONE',  ( 13.49999999999999822, 16.28000000000001535, 4.386415899144237684 ) ) ;
#16274 = CARTESIAN_POINT ( 'NONE',  ( 13.16986379959834075, -14.56874999999996589, 13.16986379960055231 ) ) ;
#16275 = CARTESIAN_POINT ( 'NONE',  ( 13.38028740620904244, 66.49273914559641696, -1.795635039658233900 ) ) ;
#16276 = CARTESIAN_POINT ( 'NONE',  ( 3.501237990040255266, 56.80573784203645715, 13.03990057735902752 ) ) ;
#16277 = CARTESIAN_POINT ( 'NONE',  ( -9.520470885617717371, 66.23000000000000398, 6.917026985038133624 ) ) ;
#16278 = CARTESIAN_POINT ( 'NONE',  ( -9.520470885617717371, 66.23000000000000398, 6.917026985038133624 ) ) ;
#16279 = CARTESIAN_POINT ( 'NONE',  ( -11.35548083115155471, 47.20349252989605304, 7.300894966903513250 ) ) ;
#16280 = CARTESIAN_POINT ( 'NONE',  ( -8.891200544363830713E-16, 46.67999999999999972, 13.50000000000000000 ) ) ;
#16281 = CARTESIAN_POINT ( 'NONE',  ( -7.999999999999776179, 0.000000000000000000, -17.32050807568887762 ) ) ;
#16282 = CARTESIAN_POINT ( 'NONE',  ( 17.21696878885094861, -99.99999999999994316, 6.677246014329758950 ) ) ;
#16283 = CARTESIAN_POINT ( 'NONE',  ( -3.863179568236954964, 56.54109641619593418, 12.93566548485912193 ) ) ;
#16284 = CARTESIAN_POINT ( 'NONE',  ( -8.043339635996302306, -56.19374999999985931, -8.043339635997654113 ) ) ;
#16285 =( BOUNDED_CURVE ( )  B_SPLINE_CURVE ( 2, ( #4292, #9704, #12336, #1718, #16388, #13646, #16568, #4474, #2857, #1630, #8638 ),
 .UNSPECIFIED., .F., .F. ) 
 B_SPLINE_CURVE_WITH_KNOTS ( ( 3, 2, 2, 2, 2, 3 ),
 ( 0.6250000000000000000, 0.6277777777777777679, 0.6333333333333333037, 0.6388888888888888395, 0.6444444444444444864, 0.6468607619886460602 ),
 .UNSPECIFIED. ) 
 CURVE ( )  GEOMETRIC_REPRESENTATION_ITEM ( )  RATIONAL_B_SPLINE_CURVE ( ( 0.9755282581475768211, 0.9755282581475768211, 1.000000000000000000, 0.9510565162951535312, 1.000000000000000000, 0.9510565162951535312, 1.000000000000000000, 0.9510565162951535312, 1.000000000000000000, 0.9787126602969342670, 0.9759426306556713282 ) ) 
 REPRESENTATION_ITEM ( '' )  );
#16286 = CARTESIAN_POINT ( 'NONE',  ( 15.00000000000000000, -100.0000000000000000, 0.000000000000000000 ) ) ;
#16287 = CARTESIAN_POINT ( 'NONE',  ( 13.48910014420235193, 33.40263309453820995, 0.7849891466346210489 ) ) ;
#16288 = CARTESIAN_POINT ( 'NONE',  ( -7.999999999999705125, 6.548268786306342903, -22.26879735319537090 ) ) ;
#16289 = CARTESIAN_POINT ( 'NONE',  ( 0.03365071246442605246, 40.17879039882647163, -13.49996849265505716 ) ) ;
#16290 = ORIENTED_EDGE ( 'NONE', *, *, #7934, .T. ) ;
#16291 = CARTESIAN_POINT ( 'NONE',  ( -5.500314997612258061, 62.48055942713471467, 12.32876052380532350 ) ) ;
#16292 = ORIENTED_EDGE ( 'NONE', *, *, #12150, .F. ) ;
#16293 = ADVANCED_FACE ( 'NONE', ( #14916 ), #3890, .F. ) ;
#16294 = CARTESIAN_POINT ( 'NONE',  ( -18.62500000000064659, -33.26562499999994316, 7.714727599197333419 ) ) ;
#16295 = CARTESIAN_POINT ( 'NONE',  ( -13.46144879879456369, 43.96558710645349066, 1.028303578921997641 ) ) ;
#16296 = CARTESIAN_POINT ( 'NONE',  ( -11.00000000000012612, 7.773118517290097174, 15.58845726811980725 ) ) ;
#16297 = CARTESIAN_POINT ( 'NONE',  ( -4.171729424061791036, 41.52999999999999403, 12.83926296998457239 ) ) ;
#16298 = CARTESIAN_POINT ( 'NONE',  ( -13.49999999999999822, 45.78000000000000114, -4.386415899144240349 ) ) ;
#16299 = CARTESIAN_POINT ( 'NONE',  ( -13.45257578124989628, 70.96919024973162493, 1.130622322280563363 ) ) ;
#16300 = CARTESIAN_POINT ( 'NONE',  ( -18.62500000000064659, -68.71562499999981810, 7.714727599197333419 ) ) ;
#16301 = CARTESIAN_POINT ( 'NONE',  ( -5.592092107590749706, 67.38298209709476794, -12.28733440995878468 ) ) ;
#16302 = CARTESIAN_POINT ( 'NONE',  ( 7.714727599200456254, -45.82187499999987779, -18.62499999999935341 ) ) ;
#16303 = CARTESIAN_POINT ( 'NONE',  ( 12.04768657887330185, 54.20515543561278093, 6.106558576545860539 ) ) ;
#16304 = CARTESIAN_POINT ( 'NONE',  ( -13.37418999445743317, 64.99429005833133033, 1.839119788055520344 ) ) ;
#16305 = ORIENTED_EDGE ( 'NONE', *, *, #5942, .T. ) ;
#16306 = CARTESIAN_POINT ( 'NONE',  ( -11.86075464149945979, 34.69129769346438508, -6.447695951845784812 ) ) ;
#16307 = AXIS2_PLACEMENT_3D ( 'NONE', #15328, #9806, #3051 ) ;
#16308 = VERTEX_POINT ( 'NONE', #10705 ) ;
#16309 = CARTESIAN_POINT ( 'NONE',  ( 13.46095473589419989, 78.46569523006924385, -1.031123768929128603 ) ) ;
#16310 = LINE ( 'NONE', #4217, #9291 ) ;
#16311 = CARTESIAN_POINT ( 'NONE',  ( -7.935043333107852703, 31.47999643740649489, -10.92183493073192402 ) ) ;
#16312 = CARTESIAN_POINT ( 'NONE',  ( 6.454605826760913878, 72.94287210141447986, -11.86071968115371611 ) ) ;
#16313 = CARTESIAN_POINT ( 'NONE',  ( 9.520470885617715595, -9.869999999999997442, 6.917026985038135400 ) ) ;
#16314 = CARTESIAN_POINT ( 'NONE',  ( 3.225258522805953376, 59.79597076863439753, 13.10906991609496863 ) ) ;
#16315 = CARTESIAN_POINT ( 'NONE',  ( -4.171729424061787483, -15.66999999999999638, -12.83926296998457417 ) ) ;
#16316 = CARTESIAN_POINT ( 'NONE',  ( 13.50000000000000000, 69.43000000000000682, 1.653273178848926867E-15 ) ) ;
#16317 = CARTESIAN_POINT ( 'NONE',  ( -12.28080000939004712, 53.13556830417786614, 5.614090485097651850 ) ) ;
#16318 = CARTESIAN_POINT ( 'NONE',  ( 3.636496289402154414, 51.82999999999999829, 11.19198476289190936 ) ) ;
#16319 = CARTESIAN_POINT ( 'NONE',  ( 2.607531440858944223E-15, 66.17999999999999261, -14.19474002721660355 ) ) ;
#16320 = CARTESIAN_POINT ( 'NONE',  ( -17.32050807568867512, 7.773118517290098062, -8.000000000000207834 ) ) ;
#16321 = AXIS2_PLACEMENT_3D ( 'NONE', #6787, #58, #5461 ) ;
#16322 = EDGE_CURVE ( 'NONE', #908, #1193, #5589, .T. ) ;
#16323 = CARTESIAN_POINT ( 'NONE',  ( 9.112504148662578629, 69.03424743680851350, 9.973291273079063046 ) ) ;
#16324 = CARTESIAN_POINT ( 'NONE',  ( -5.242085789724583833, 37.36954959029712597, -12.44118853238696154 ) ) ;
#16325 = CARTESIAN_POINT ( 'NONE',  ( 2.530949507919612707, 35.77097839341501384, 13.26251326736510094 ) ) ;
#16326 = CARTESIAN_POINT ( 'NONE',  ( -13.16986379959834252, -13.49374999999998792, -13.16986379960055409 ) ) ;
#16327 = CARTESIAN_POINT ( 'NONE',  ( -11.10711687597100727, 74.21892446219855799, 7.674797575374098457 ) ) ;
#16328 = CARTESIAN_POINT ( 'NONE',  ( -13.38715452818623142, 76.86871122637566600, -1.752948765687992294 ) ) ;
#16329 = CARTESIAN_POINT ( 'NONE',  ( -0.6924984764758839173, 8.027888383433452901, -18.11551784069753879 ) ) ;
#16330 = CYLINDRICAL_SURFACE ( 'NONE', #4117, 13.50000000000000000 ) ;
#16331 = CARTESIAN_POINT ( 'NONE',  ( -19.00000000000001776, 0.000000000000000000, 1.732050807568674466 ) ) ;
#16332 = PRESENTATION_STYLE_ASSIGNMENT (( #11052 ) ) ;
#16333 = CARTESIAN_POINT ( 'NONE',  ( -7.272992578804307939, 0.4799999999999978728, -10.01041549318726886 ) ) ;
#16334 = CARTESIAN_POINT ( 'NONE',  ( -3.636496289402153081, 47.32999999999999829, -11.19198476289190936 ) ) ;
#16335 = CARTESIAN_POINT ( 'NONE',  ( 13.50000000000000355, -14.41999999999999638, -4.386415899144233244 ) ) ;
#16336 = CARTESIAN_POINT ( 'NONE',  ( -11.88952341483570585, 40.69343732765294419, -6.394472622149963925 ) ) ;
#16337 = CARTESIAN_POINT ( 'NONE',  ( -2.782897275306619900, 34.28006271705798014, -13.21006040336913578 ) ) ;
#16338 = CARTESIAN_POINT ( 'NONE',  ( 13.02980635443139867, 75.30032106848673834, 3.643481502864720500 ) ) ;
#16339 = CARTESIAN_POINT ( 'NONE',  ( 3.073853547173910350, -1.028534069218512171E-14, -14.38353912379420230 ) ) ;
#16340 = CARTESIAN_POINT ( 'NONE',  ( -3.636496289402155746, 33.52999999999999403, 11.19198476289190936 ) ) ;
#16341 = CARTESIAN_POINT ( 'NONE',  ( -8.912260708675086462, 41.33526359048111232, 10.14439829438506457 ) ) ;
#16342 = CARTESIAN_POINT ( 'NONE',  ( 10.08123987682633249, 51.77650836596966144, -8.978842906595179585 ) ) ;
#16343 = CONICAL_SURFACE ( 'NONE', #1959, 9.500000000000021316, 0.7853981633974504994 ) ;
#16344 = EDGE_CURVE ( 'NONE', #5443, #4638, #14743, .T. ) ;
#16345 = CARTESIAN_POINT ( 'NONE',  ( 6.542315702985624704, 44.92083719594266000, 11.80973987326741081 ) ) ;
#16346 = CYLINDRICAL_SURFACE ( 'NONE', #17383, 13.50000000000000000 ) ;
#16347 = CARTESIAN_POINT ( 'NONE',  ( -13.50000000000000000, 4.930000000000004157, -3.469446951953614189E-15 ) ) ;
#16348 = AXIS2_PLACEMENT_3D ( 'NONE', #14225, #11596, #6386 ) ;
#16349 = CARTESIAN_POINT ( 'NONE',  ( -4.171729424061787483, 57.32999999999999829, -12.83926296998457417 ) ) ;
#16350 = CARTESIAN_POINT ( 'NONE',  ( -9.678251426474608010, 49.56251328237163989, -9.415881064490173813 ) ) ;
#16351 = CARTESIAN_POINT ( 'NONE',  ( 13.48030235938352561, 63.40470212201357469, 0.7310520173840249214 ) ) ;
#16352 = CARTESIAN_POINT ( 'NONE',  ( 10.66756771982902308, 42.11545174721990037, 8.273639169023212503 ) ) ;
#16353 = CARTESIAN_POINT ( 'NONE',  ( 5.371075548745484873, 48.98509448818010981, -12.38750806412678429 ) ) ;
#16354 = ORIENTED_EDGE ( 'NONE', *, *, #10137, .F. ) ;
#16355 = CARTESIAN_POINT ( 'NONE',  ( -1.104539697211379901, 70.21968188907926844, -13.46197618054497447 ) ) ;
#16356 = CARTESIAN_POINT ( 'NONE',  ( -11.37499999999960387, -7.284374999999982059, -4.711679271994911211 ) ) ;
#16357 = ORIENTED_EDGE ( 'NONE', *, *, #10800, .F. ) ;
#16358 = CARTESIAN_POINT ( 'NONE',  ( -8.704009495233664850, 43.51509674902774805, -10.31941033300555333 ) ) ;
#16359 = CARTESIAN_POINT ( 'NONE',  ( -7.499999999999999112, 103.9536021580775156, 9.261711852864909389 ) ) ;
#16360 = CARTESIAN_POINT ( 'NONE',  ( 13.24512690636890611, 60.52253756231457515, -2.622165425226990809 ) ) ;
#16361 = CARTESIAN_POINT ( 'NONE',  ( 13.49999999999999822, 13.28000000000001002, 4.386415899144237684 ) ) ;
#16362 = LINE ( 'NONE', #9679, #2856 ) ;
#16363 = CARTESIAN_POINT ( 'NONE',  ( 13.49371366599027944, 66.41232310859372490, 0.5032188625160722850 ) ) ;
#16364 = CARTESIAN_POINT ( 'NONE',  ( 10.68173734215865345, 57.11625071965492140, 8.255346062962116704 ) ) ;
#16365 = CARTESIAN_POINT ( 'NONE',  ( 3.636496289402154414, 60.82999999999999829, 11.19198476289190936 ) ) ;
#16366 = CARTESIAN_POINT ( 'NONE',  ( -11.76794919243112325, 65.78000000000001535, -3.823638476888998827 ) ) ;
#16367 = CARTESIAN_POINT ( 'NONE',  ( -7.109540715892270768, 47.41573464837242824, 11.47625667131351612 ) ) ;
#16368 = B_SPLINE_CURVE_WITH_KNOTS ( 'NONE', 3,
 ( #1731, #12530, #4574, #414, #5822, #7408, #11206, #16581, #12790, #9895, #15243, #588, #3141, #8566, #9981, #7317, #5998, #676 ),
 .UNSPECIFIED., .F., .F.,
 ( 4, 2, 2, 2, 2, 2, 2, 2, 4 ),
 ( 2.344180274388505961E-07, 0.0005273255548235156187, 0.001054416691619592403, 0.001581507828415669187, 0.002108598965211746189, 0.002635690102007825792, 0.003162781238803905395, 0.003689872375599984999, 0.004216963512396064602 ),
 .UNSPECIFIED. ) ;
#16369 = LINE ( 'NONE', #17436, #3629 ) ;
#16370 = CARTESIAN_POINT ( 'NONE',  ( 12.00000000000006217, 8.413974596215602730, 3.899036354794897186 ) ) ;
#16371 = ADVANCED_FACE ( 'NONE', ( #16156, #4065 ), #13513, .T. ) ;
#16372 = B_SPLINE_CURVE_WITH_KNOTS ( 'NONE', 3,
 ( #14953, #8452, #13547, #1618, #4279, #13635, #15038, #13891, #2932, #1437, #6855, #9866, #10914, #7117, #7035, #12233, #13806, #2843, #124, #16283, #12587, #5530, #8541, #5885, #1704, #389, #11265, #300, #12413, #5795, #4099, #5710, #11179, #16554, #8274, #15217, #1528, #6944, #4461, #3113, #11092, #1790, #12323, #16464, #4368, #216, #9777, #4804, #4548, #8710, #1956, #10206, #13016, #6309, #2124, #6056, #9953, #646, #4719, #16811, #16986, #3385, #897, #16726, #15560, #15301, #8798, #11439, #14070, #10121, #8967, #15474, #3205, #8625, #4890, #5970, #7550, #2043, #13977, #8884, #15389, #10291, #14155, #3470, #7467, #3296, #14239, #1872, #16901, #6144, #813, #16642, #12928, #2211, #15643, #3553, #7288, #11523, #12673, #563, #12847, #6224, #11610, #736, #7639, #14323, #11351, #4633, #10039, #7380, #12758, #13355, #17246, #10716, #7724, #5070, #11954, #3729, #14494, #16081, #9147, #4975, #13275, #6656, #3641, #17158, #10378, #9405, #14753, #2642, #6574, #10631, #13189, #3901, #1325, #1163, #15910, #8073, #15732, #13100, #2381, #13438, #11695, #10464, #1074, #15824, #9319, #3989, #9054, #14408, #2296, #7817, #17071, #12037, #17334, #5331, #5158, #987, #6399, #6488, #15996, #17416, #11782, #11871, #2467, #7900, #10551, #3819, #14669, #9233, #14587, #5245, #2557, #7987, #1243, #11065, #8424, #16258, #2731, #4164, #15095 ),
 .UNSPECIFIED., .F., .F.,
 ( 4, 2, 2, 2, 2, 1, 2, 2, 2, 2, 2, 2, 2, 2, 2, 1, 2, 2, 2, 2, 1, 2, 2, 1, 1, 1, 2, 2, 2, 1, 2, 2, 1, 1, 2, 2, 2, 2, 1, 1, 1, 2, 2, 2, 1, 1, 2, 2, 1, 1, 1, 2, 1, 2, 2, 1, 2, 2, 2, 2, 1, 2, 2, 2, 2, 2, 2, 1, 2, 2, 2, 2, 1, 1, 2, 2, 2, 2, 2, 2, 1, 1, 2, 2, 2, 1, 2, 2, 1, 2, 2, 2, 2, 2, 2, 2, 2, 2, 2, 2, 2, 1, 1, 2, 4 ),
 ( 0.4755055480612112584, 0.4764246321120116368, 0.4768841741374118537, 0.4769416168905868947, 0.4769990596437618802, 0.4771139451501119622, 0.4773437161628120706, 0.4778032581882122320, 0.4780330292009123405, 0.4781479147072624225, 0.4782628002136124490, 0.4791818842644128829, 0.4794116552771129913, 0.4794690980302880323, 0.4794978194068755251, 0.4795265407834630178, 0.4796414262898130998, 0.4801009683152132612, 0.4810200523660136396, 0.4819391364168140179, 0.4819678577934015107, 0.4819822184816953126, 0.4819965791699890589, 0.4820540219231640444, 0.4821689074295141264, 0.4823986784422141794, 0.4828582204676143408, 0.4837773045184146081, 0.4842368465438147696, 0.4844666175565148780, 0.4844953389331023708, 0.4845096996213961171, 0.4845240603096898635, 0.4845815030628649045, 0.4846963885692149310, 0.4865345566708156877, 0.4869940986962159046, 0.4870228200728033974, 0.4870515414493908901, 0.4871089842025659311, 0.4872238697089160131, 0.4874536407216160661, 0.4883727247724164444, 0.4892918088232168228, 0.4894066943295668493, 0.4894641370827418903, 0.4894928584593293830, 0.4895072191476231294, 0.4895215798359168757, 0.4897513508486169842, 0.4902108928740171456, 0.4906704348994173626, 0.4907278776525924036, 0.4907422383408861499, 0.4907565990291798963, 0.4907853204057673890, 0.4909002059121174710, 0.4911299769248175795, 0.4915895189502177409, 0.4918192899629178494, 0.4919341754692679314, 0.4919916182224429169, 0.4920490609756179579, 0.4938872290772187701, 0.4943467711026189870, 0.4944616566089690135, 0.4945190993621440545, 0.4945765421153190955, 0.4948063131280192040, 0.4957253971788195823, 0.4957541185554070751, 0.4957684792437008769, 0.4957828399319946233, 0.4958402826851696088, 0.4959551681915196908, 0.4961849392042197437, 0.4966444812296199052, 0.4968742522423200136, 0.4969891377486700401, 0.4970178591252575329, 0.4970465805018450811, 0.4971040232550200666, 0.4975635652804201170, 0.4984826493312203288, 0.4994017333820204851, 0.4994591761351955261, 0.4994878975117830189, 0.4995166188883705116, 0.4996315043947205381, 0.4998612754074205911, 0.5003208174328206415, 0.5012399014836208533, 0.5016994435090209592, 0.5019292145217210122, 0.5020441000280710941, 0.5021589855344210651, 0.5030780695852212769, 0.5039971536360214888, 0.5044566956614215947, 0.5045141384145965802, 0.5045284991028903265, 0.5045428597911841839, 0.5045715811677716767, 0.5046864666741216476, 0.5049162376868217006 ),
 .UNSPECIFIED. ) ;
#16373 = CARTESIAN_POINT ( 'NONE',  ( 8.825897884691713102, -99.99999999999998579, 14.84509086929686283 ) ) ;
#16374 = CARTESIAN_POINT ( 'NONE',  ( -9.062685027414643102, 10.00000000000000000, -8.691113669179740597 ) ) ;
#16375 = CARTESIAN_POINT ( 'NONE',  ( -11.37500000000000000, -91.57499999999977547, -9.545674412382054647E-13 ) ) ;
#16376 = PRODUCT_DEFINITION_FORMATION_WITH_SPECIFIED_SOURCE ( 'ANY', '', #6700, .NOT_KNOWN. ) ;
#16377 = CARTESIAN_POINT ( 'NONE',  ( 13.30970590930321507, 33.35061697494153776, 2.259477746023484279 ) ) ;
#16378 = CARTESIAN_POINT ( 'NONE',  ( 4.012506912825325678, 10.00000000000000178, 12.61441303195674735 ) ) ;
#16379 = FACE_OUTER_BOUND ( 'NONE', #10363, .T. ) ;
#16380 = CARTESIAN_POINT ( 'NONE',  ( 11.76794919243112325, 23.28000000000000114, 3.823638476888996163 ) ) ;
#16381 = VERTEX_POINT ( 'NONE', #15353 ) ;
#16382 = CARTESIAN_POINT ( 'NONE',  ( -5.714934635204341085, 62.47224522950935466, 12.23094497409742765 ) ) ;
#16383 = ORIENTED_EDGE ( 'NONE', *, *, #16200, .F. ) ;
#16384 = CARTESIAN_POINT ( 'NONE',  ( -13.49672419826743486, 40.91718416035435268, -0.3692389318145620769 ) ) ;
#16385 = CARTESIAN_POINT ( 'NONE',  ( -11.76794919243112325, -13.91999999999999815, 3.823638476888994386 ) ) ;
#16386 = CARTESIAN_POINT ( 'NONE',  ( -7.714727599200466912, -35.34687499999993321, 18.62499999999935341 ) ) ;
#16387 = CARTESIAN_POINT ( 'NONE',  ( -13.39191227960274411, 43.99185072783001260, 1.775942202619223531 ) ) ;
#16388 = CARTESIAN_POINT ( 'NONE',  ( 10.92172942406179104, 0.7300000000000084199, -7.935100905948385908 ) ) ;
#16389 = CARTESIAN_POINT ( 'NONE',  ( -13.49999999999999822, 35.07999999999999119, 4.386415899144235908 ) ) ;
#16390 = CARTESIAN_POINT ( 'NONE',  ( 13.50000000000000000, 44.42999999999999972, 1.653273178848926867E-15 ) ) ;
#16391 =( BOUNDED_CURVE ( )  B_SPLINE_CURVE ( 2, ( #2100, #2361, #6637, #13165, #7615, #12991, #2535, #3615, #17310, #17224, #874, #6550, #13077 ),
 .UNSPECIFIED., .F., .F. ) 
 B_SPLINE_CURVE_WITH_KNOTS ( ( 3, 2, 2, 2, 2, 2, 3 ),
 ( 0.5694444444444444198, 0.5722222222222221877, 0.5777777777777777235, 0.5833333333333333703, 0.5888888888888889062, 0.5944444444444444420, 0.5972222222222222099 ),
 .UNSPECIFIED. ) 
 CURVE ( )  GEOMETRIC_REPRESENTATION_ITEM ( )  RATIONAL_B_SPLINE_CURVE ( ( 0.9755282581475768211, 0.9755282581475768211, 1.000000000000000000, 0.9510565162951535312, 1.000000000000000000, 0.9510565162951535312, 1.000000000000000000, 0.9510565162951535312, 1.000000000000000000, 0.9510565162951535312, 1.000000000000000000, 0.9755282581475768211, 0.9755282581475768211 ) ) 
 REPRESENTATION_ITEM ( '' )  );
#16392 = EDGE_CURVE ( 'NONE', #11282, #11898, #5015, .T. ) ;
#16393 = CARTESIAN_POINT ( 'NONE',  ( 7.714727599200456254, -29.17187499999991118, -18.62499999999935341 ) ) ;
#16394 = CARTESIAN_POINT ( 'NONE',  ( -10.35534497003228616, 67.59815324688858595, -8.661887587482873130 ) ) ;
#16395 = CARTESIAN_POINT ( 'NONE',  ( -7.714727599197334307, -64.55312499999983800, -18.62500000000064659 ) ) ;
#16396 = CARTESIAN_POINT ( 'NONE',  ( 12.99745066060657983, 54.56037337467130044, -3.649188683310558012 ) ) ;
#16397 = CARTESIAN_POINT ( 'NONE',  ( -0.6906333296155144907, 64.20483233361511566, -13.48257629628379739 ) ) ;
#16398 = ORIENTED_EDGE ( 'NONE', *, *, #3751, .F. ) ;
#16399 = PLANE ( 'NONE',  #2117 ) ;
#16400 = CARTESIAN_POINT ( 'NONE',  ( -13.48149335069471277, 34.90545412603139397, -0.7087578777626947213 ) ) ;
#16401 = ORIENTED_EDGE ( 'NONE', *, *, #10680, .T. ) ;
#16402 = CARTESIAN_POINT ( 'NONE',  ( 13.40590469924962136, 78.37451624811531303, 1.591240554925627215 ) ) ;
#16403 = CARTESIAN_POINT ( 'NONE',  ( -12.50000000000000000, -18.00000000000000355, -2.204364238465235822E-15 ) ) ;
#16404 = CARTESIAN_POINT ( 'NONE',  ( -24.73863375370603634, 0.000000000000000000, 7.999999999999761080 ) ) ;
#16405 = CARTESIAN_POINT ( 'NONE',  ( -8.343458848123582072, 37.37999999999999545, 11.48378591275253768 ) ) ;
#16406 = CARTESIAN_POINT ( 'NONE',  ( 3.355142272266856018, 73.05936141215188684, -13.07645859584844317 ) ) ;
#16407 = PLANE ( 'NONE',  #11430 ) ;
#16408 = CARTESIAN_POINT ( 'NONE',  ( 13.50000000000000000, -19.56999999999999673, 1.734723475976807094E-15 ) ) ;
#16409 = CARTESIAN_POINT ( 'NONE',  ( -8.691771469529815392E-16, 62.67999999999999972, 14.19474002721660355 ) ) ;
#16410 = CARTESIAN_POINT ( 'NONE',  ( -13.08971297670988676, 53.04813283155247916, 3.315942555628902166 ) ) ;
#16411 = CARTESIAN_POINT ( 'NONE',  ( -11.76794919243112325, 36.08000000000000540, 3.823638476888994386 ) ) ;
#16412 = CARTESIAN_POINT ( 'NONE',  ( 8.050216715958701030, -18.96812692063824812, 8.940658242654158983 ) ) ;
#16413 = CARTESIAN_POINT ( 'NONE',  ( 2.607531440858944223E-15, 54.17999999999999261, -14.19474002721660355 ) ) ;
#16414 = CARTESIAN_POINT ( 'NONE',  ( 2.431254415941702884, 50.76746427736173928, 13.28206675338410570 ) ) ;
#16415 = CARTESIAN_POINT ( 'NONE',  ( 12.74062673367197540, 69.26888048504336837, 4.464895979421934946 ) ) ;
#16416 = CARTESIAN_POINT ( 'NONE',  ( -13.16986379960055231, -10.40624999999997513, 13.16986379959834252 ) ) ;
#16417 = CARTESIAN_POINT ( 'NONE',  ( -4.171729424061787483, 72.33000000000001251, -12.83926296998457417 ) ) ;
#16418 = CARTESIAN_POINT ( 'NONE',  ( -18.62499999999935341, -47.83437499999990195, -7.714727599200458030 ) ) ;
#16419 = CARTESIAN_POINT ( 'NONE',  ( -13.20956847790360733, 74.02888101833143253, 2.796753555545153258 ) ) ;
#16420 = CARTESIAN_POINT ( 'NONE',  ( -4.859696658499787603, 76.35516489890081004, -12.59554570565296139 ) ) ;
#16421 = CARTESIAN_POINT ( 'NONE',  ( -3.256378952507587687, 79.29685528557507723, -13.10825059591972241 ) ) ;
#16422 = DIRECTION ( 'NONE',  ( 0.000000000000000000, 0.000000000000000000, -1.000000000000000000 ) ) ;
#16423 = CARTESIAN_POINT ( 'NONE',  ( 3.590940523863186851, 80.92999999999996419, 12.80902731135801886 ) ) ;
#16424 =( NAMED_UNIT ( * ) SI_UNIT ( $, .STERADIAN. ) SOLID_ANGLE_UNIT ( ) );
#16425 = CARTESIAN_POINT ( 'NONE',  ( -7.272992578804307939, -2.520000000000001794, -10.01041549318726886 ) ) ;
#16426 = CARTESIAN_POINT ( 'NONE',  ( 7.272992578804311492, 46.87999999999998835, -10.01041549318726886 ) ) ;
#16427 = CARTESIAN_POINT ( 'NONE',  ( -4.171729424061791036, 2.530000000000004690, 12.83926296998457239 ) ) ;
#16428 = AXIS2_PLACEMENT_3D ( 'NONE', #12501, #13803, #15036 ) ;
#16429 = CARTESIAN_POINT ( 'NONE',  ( -0.4449892875956310556, 32.66412856956223720, 13.50000000012790657 ) ) ;
#16430 = CARTESIAN_POINT ( 'NONE',  ( 13.34255314625656474, 75.35788651830209517, 2.057478645647980109 ) ) ;
#16431 = EDGE_CURVE ( 'NONE', #16381, #10808, #9031, .T. ) ;
#16432 = CARTESIAN_POINT ( 'NONE',  ( 3.144316449151975501, -1.028534069218507438E-14, -14.16943933260104949 ) ) ;
#16433 =( NAMED_UNIT ( * ) SI_UNIT ( $, .STERADIAN. ) SOLID_ANGLE_UNIT ( ) );
#16434 = CARTESIAN_POINT ( 'NONE',  ( -6.368869478743532930, 41.44634379311723649, 11.90564925343862868 ) ) ;
#16435 = CARTESIAN_POINT ( 'NONE',  ( 3.227881820449359562, 52.06437088216431874, -13.11849352263842761 ) ) ;
#16436 = CARTESIAN_POINT ( 'NONE',  ( -1.816329563374412759, 38.61463869457227815, 13.37757954458849241 ) ) ;
#16437 = DIRECTION ( 'NONE',  ( 0.000000000000000000, 0.000000000000000000, -1.000000000000000000 ) ) ;
#16438 = CARTESIAN_POINT ( 'NONE',  ( -5.441113646577662166, 5.918584287042170544, 25.42428528562851042 ) ) ;
#16439 = CARTESIAN_POINT ( 'NONE',  ( -1.900613283894366567, 1.737093173895315257, 12.00000000000004974 ) ) ;
#16440 = CARTESIAN_POINT ( 'NONE',  ( -11.16732475769975963, 49.64467603628539649, -7.585655084846200324 ) ) ;
#16441 = CARTESIAN_POINT ( 'NONE',  ( 9.616125506160093650, 63.05947077844894721, 9.475237748159102580 ) ) ;
#16442 = CARTESIAN_POINT ( 'NONE',  ( 12.14686625650739416, 42.21335745758226921, 5.893900887576004166 ) ) ;
#16443 = CARTESIAN_POINT ( 'NONE',  ( 5.822740267050442675, 48.96792138070764366, -12.17985001218392327 ) ) ;
#16444 = EDGE_LOOP ( 'NONE', ( #16487, #197 ) ) ;
#16445 = CARTESIAN_POINT ( 'NONE',  ( -11.76794919243112325, 71.92999999999999261, -2.882316262207890869E-15 ) ) ;
#16446 = CARTESIAN_POINT ( 'NONE',  ( -2.234432163248517789, 70.26033055681520523, -13.31411821497241199 ) ) ;
#16447 = CARTESIAN_POINT ( 'NONE',  ( -4.711679271993003404, -55.15312499999986784, -11.37500000000039435 ) ) ;
#16448 = CARTESIAN_POINT ( 'NONE',  ( -4.171729424061791036, 8.530000000000010019, 12.83926296998457239 ) ) ;
#16449 = VERTEX_POINT ( 'NONE', #16218 ) ;
#16450 = CARTESIAN_POINT ( 'NONE',  ( -4.039390320560676706, 43.32524183929319150, -12.88154992939627874 ) ) ;
#16451 = DIRECTION ( 'NONE',  ( 0.000000000000000000, 0.000000000000000000, -1.000000000000000000 ) ) ;
#16452 = CARTESIAN_POINT ( 'NONE',  ( 6.713091215227763975, 60.93229263216861824, -11.71350425076765234 ) ) ;
#16453 = CARTESIAN_POINT ( 'NONE',  ( -13.50000000000000000, 2.930000000000001936, -3.469446951953614189E-15 ) ) ;
#16454 = CIRCLE ( 'NONE', #11948, 1.999999999999998224 ) ;
#16455 = CARTESIAN_POINT ( 'NONE',  ( -13.16986379960055231, -10.40624999999997513, 13.16986379959834252 ) ) ;
#16456 = CARTESIAN_POINT ( 'NONE',  ( 12.41472406366220937, 66.62365169156784361, -5.310316743964890840 ) ) ;
#16457 = CARTESIAN_POINT ( 'NONE',  ( 9.085652227950054893, 57.03291504710205118, 9.999132570447487822 ) ) ;
#16458 = CARTESIAN_POINT ( 'NONE',  ( 7.272992578804308828, 54.98000000000000398, 10.01041549318726709 ) ) ;
#16459 = CARTESIAN_POINT ( 'NONE',  ( 2.272985001014427788E-15, 65.18000000000000682, -12.37355403259654985 ) ) ;
#16460 = CARTESIAN_POINT ( 'NONE',  ( -13.48866837566228050, 46.90290234888265530, -0.7789067716198110336 ) ) ;
#16461 = CARTESIAN_POINT ( 'NONE',  ( 15.00000000000000000, 0.000000000000000000, 1.256933281983527907E-12 ) ) ;
#16462 = FACE_OUTER_BOUND ( 'NONE', #7042, .T. ) ;
#16463 = CARTESIAN_POINT ( 'NONE',  ( 6.184124730272909432, 30.95379574339498419, -12.00166303903518461 ) ) ;
#16464 = CARTESIAN_POINT ( 'NONE',  ( -8.721356837196914569, 56.34409543140491650, 10.30502666443673654 ) ) ;
#16465 = CARTESIAN_POINT ( 'NONE',  ( 8.043339635997654113, -68.68124999999983515, -8.043339635996304082 ) ) ;
#16466 = DIRECTION ( 'NONE',  ( 0.000000000000000000, 1.000000000000000000, 0.000000000000000000 ) ) ;
#16467 = CARTESIAN_POINT ( 'NONE',  ( 4.319503133742830236, 32.83532678599706855, 12.79097160616992745 ) ) ;
#16468 = CARTESIAN_POINT ( 'NONE',  ( -17.32050807568867512, 0.000000000000000000, -8.000000000000207834 ) ) ;
#16469 = CARTESIAN_POINT ( 'NONE',  ( 1.040369979270597378, 40.14266547395921236, -13.46226468211543725 ) ) ;
#16470 = ORIENTED_EDGE ( 'NONE', *, *, #5455, .T. ) ;
#16471 = CARTESIAN_POINT ( 'NONE',  ( -4.171729424061787483, 42.32999999999999829, -12.83926296998457417 ) ) ;
#16472 = ORIENTED_EDGE ( 'NONE', *, *, #1742, .F. ) ;
#16473 = CARTESIAN_POINT ( 'NONE',  ( 11.76794919243112680, -15.41999999999999993, -3.823638476888993942 ) ) ;
#16474 = CARTESIAN_POINT ( 'NONE',  ( -7.714727599200466912, -68.64687499999988063, 18.62499999999935341 ) ) ;
#16475 = CARTESIAN_POINT ( 'NONE',  ( -13.01704944681739384, 44.05820777106878694, 3.585442433228816839 ) ) ;
#16476 = EDGE_CURVE ( 'NONE', #1252, #2386, #16803, .T. ) ;
#16477 = CARTESIAN_POINT ( 'NONE',  ( -17.32050807568867512, 0.000000000000000000, -8.000000000000207834 ) ) ;
#16478 = CARTESIAN_POINT ( 'NONE',  ( -8.343458848123582072, 32.37999999999999545, 11.48378591275254124 ) ) ;
#16479 = CARTESIAN_POINT ( 'NONE',  ( -4.171729424061791036, 49.53000000000000114, 12.83926296998457239 ) ) ;
#16480 = CARTESIAN_POINT ( 'NONE',  ( -6.265920072760685855, 46.40952468282172561, -11.95780131475176411 ) ) ;
#16481 = CARTESIAN_POINT ( 'NONE',  ( -5.840637679356421863, 67.39265420351648572, -12.17211919009271170 ) ) ;
#16482 = CARTESIAN_POINT ( 'NONE',  ( -18.62500000000000000, -51.02499999999986358, -1.562973063126292757E-12 ) ) ;
#16483 = CARTESIAN_POINT ( 'NONE',  ( 10.70096191381189854, 54.74267225910909929, -8.231670366690693186 ) ) ;
#16484 = CARTESIAN_POINT ( 'NONE',  ( -5.858038622988929411, 64.39335049776337883, -12.16278876361409367 ) ) ;
#16485 = ORIENTED_EDGE ( 'NONE', *, *, #14233, .T. ) ;
#16486 = CARTESIAN_POINT ( 'NONE',  ( -13.47158887085881673, 34.89975520542590459, -0.8754049196653456155 ) ) ;
#16487 = ORIENTED_EDGE ( 'NONE', *, *, #15264, .T. ) ;
#16488 = CARTESIAN_POINT ( 'NONE',  ( 12.90972652943405841, 78.57172280611223414, -3.953148085708793502 ) ) ;
#16489 = CARTESIAN_POINT ( 'NONE',  ( 1.732050807568740858, 0.000000000000000000, 19.00000000000000355 ) ) ;
#16490 = EDGE_CURVE ( 'NONE', #16817, #12936, #504, .T. ) ;
#16491 = AXIS2_PLACEMENT_3D ( 'NONE', #13406, #8219, #13580 ) ;
#16492 = CARTESIAN_POINT ( 'NONE',  ( 7.500000000000001776, -24.66999453389980346, 8.557281619885985791 ) ) ;
#16493 = CARTESIAN_POINT ( 'NONE',  ( 3.408135647905105703, 73.05745548237557330, -13.06274704958987520 ) ) ;
#16494 = CARTESIAN_POINT ( 'NONE',  ( 3.048566704048218057, 79.07038407013068593, -13.15904929974419346 ) ) ;
#16495 = CARTESIAN_POINT ( 'NONE',  ( -10.92172942406179104, -11.76999999999999602, 7.935100905948385908 ) ) ;
#16496 =( BOUNDED_SURFACE ( )  B_SPLINE_SURFACE ( 3, 2, ( 
 ( #11940, #13510, #14913, #13598, #6729, #12025, #3888, #8147, #9563, #5233, #10618, #14656, #6644, #4151, #10874, #9631, #2806, #14740, #1149, #13262, #5403, #8238, #12107, #1494, #16071, #4061, #1402, #13425, #2544, #10787, #7972, #6818, #13341, #17404, #5319, #3977, #16153, #12195, #10703, #9389, #14824, #2629, #88, #8061, #1314, #14450, #7588, #15598, #15773, #7938, #11648, #5110, #4841, #3683, #938, #3591, #17111, #3856, #10415, #10245, #3506, #17285, #850, #14533, #2337, #8919, #3772, #10330, #14278, #6261, #14622, #1201, #9003, #10502, #2164, #12968, #10588, #4929, #9185, #6349, #7851, #13310, #13056, #13226, #2418, #15684, #5198, #11565, #14360, #1115, #6529, #9097, #2508, #1028, #16939, #11907, #7770 ),
 ( #11733, #17025, #15950, #2249, #7677, #6439, #9270, #5016, #13141, #11822, #17202, #15865, #16034, #12075, #17374, #4295, #9708, #15052, #1456, #3942, #4118, #9532, #5550, #4029, #8293, #12161, #5639, #2595, #17454, #6875, #16118, #9443, #11021, #14791, #5368, #16393, #1368, #2683, #2861, #10754, #8114, #8024, #14876, #13480, #13392, #6783, #1281, #1544, #6695, #4207, #13565, #52, #5288, #10670, #14971, #2951, #8380, #2772, #5457, #10840, #9620, #13735, #9357, #14706, #16207, #8203, #6612, #6963, #12249, #233, #144, #11992, #10933, #16300, #13649, #12341, #8951, #4874, #15458, #3369, #10277, #630, #6129, #12653, #14309, #12742, #8783, #12571, #5867, #14139, #16625, #4528, #7183, #10191, #14053, #458, #9935 ),
 ( #15544, #11246, #3456, #15284, #799, #5952, #15628, #2108, #11508, #8871, #16710, #3185, #4615, #14224, #3536, #7270, #2027, #7452, #8693, #8607, #3276, #12915, #11424, #16884, #13959, #1856, #543, #7535, #12832, #11332, #719, #1940, #4790, #10022, #6209, #11595, #15370, #16972, #7363, #6041, #16796, #4702, #10107, #972, #6385, #15984, #3887, #11858, #5232, #5143, #13001, #11939, #11768, #883, #9040, #5318, #9388, #17144, #1148, #6295, #10365, #1231, #13087, #17320, #9132, #9304, #16070, #3714, #14655, #10617, #5053, #13340, #3976, #10451, #2543, #7971, #6472, #10702, #9219, #2196, #6643, #10535, #6559, #15810, #12024, #7803, #17403, #15719, #14481, #2454, #2370, #13174, #7624, #1060, #17233, #11681, #15898 ),
 ( #3806, #3623, #14570, #7709, #14393, #7884, #2282, #17057, #13261, #4962, #4484, #10873, #8060, #1313, #5908, #12699, #16751, #412, #87, #10786, #12611, #7314, #12106, #13424, #6728, #13509, #14004, #15326, #16579, #8650, #3047, #2628, #14739, #4393, #13917, #16243, #16152, #4659, #586, #5402, #6817, #11379, #12194, #11287, #8477, #14956, #7225, #1811, #4060, #1401, #9803, #9476, #15241, #14823, #502, #5492, #9893, #13828, #5820, #2717, #8146, #1728, #15149, #7142, #8564, #12528, #11204, #3139, #16665, #4572, #5997, #9979, #3230, #1897, #15764, #16842, #3412, #11466, #840, #15500, #8994, #11551, #2240, #17193, #4920, #3496, #14351, #8737, #6086, #2068, #7579, #3674, #8825, #762, #14096, #7759, #674 ),
 ( #14183, #9088, #10407, #11637, #14441, #15589, #15416, #10066, #16927, #7668, #6170, #4745, #11816, #13133, #10150, #7492, #6432, #12873, #6339, #8911, #3323, #13047, #929, #1981, #4830, #10234, #7406, #10318, #12788, #11725, #14267, #17016, #2155, #12957, #6251, #15673, #3580, #17101, #5008, #2329, #1021, #9351, #11986, #14616, #10664, #14869, #3935, #15858, #3765, #10835, #11901, #8108, #8019, #9177, #14786, #3848, #14525, #17278, #8196, #12243, #2500, #4023, #2412, #13218, #4111, #15941, #2676, #17367, #1359, #1449, #6607, #6774, #13473, #9264, #16199, #6868, #7930, #12155, #45, #14700, #13559, #12070, #5103, #5450, #13387, #9437, #13303, #9525, #16029, #2763, #1105, #1195, #5362, #5281, #2588, #10495, #1276 ),
 ( #6688, #7845, #17447, #6521, #10748, #10580, #5192, #16112, #16649, #227, #13644, #15227, #7127, #13730, #10926, #4202, #8550, #15312, #1882, #3032, #2945, #1538, #3124, #9962, #14963, #16294, #9612, #16386, #4557, #487, #1716, #11273, #5719, #5542, #136, #7046, #16566, #1627, #6956, #7298, #3215, #8287, #9701, #13987, #15048, #13902, #11101, #2853, #9876, #4472, #12333, #4290, #12425, #5632, #399, #11014, #1798, #8374, #12515, #16474, #8463, #311, #4380, #9788, #15135, #13815, #11190, #5805, #7210, #12596, #5893, #8636, #4989, #11533, #5980, #11362, #910, #1966, #15654, #15569, #16737, #4902, #11449, #4643, #7391, #15745, #2309, #4730, #11621, #10049, #3306, #11707, #6066, #10301, #2054, #8978, #9068 ),
 ( #16823, #6321, #14421, #15484, #3564, #14334, #16911, #3656, #2135, #12683, #13028, #3480, #16996, #10131, #2223, #747, #17084, #8719, #3395, #12939, #8808, #14165, #10391, #7477, #12857, #573, #6156, #4814, #7652, #10216, #8894, #15399, #14249, #14079, #12768, #657, #7561, #823, #6234, #14599, #4000, #4086, #9246, #9416, #5342, #11884, #1336, #9502, #10563, #17427, #10727, #11967, #10813, #14681, #14849, #8085, #10644, #6666, #5171, #14764, #13287, #6752, #3743, #1087, #7998, #17259, #15923, #12132, #3831, #6501, #21, #2479, #7912, #2656, #1175, #6586, #9159, #16008, #13201, #13450, #1000, #5424, #7829, #14506, #16092, #2568, #17347, #6413, #11796, #16176, #7737, #13113, #3914, #5258, #2394, #17173, #5083 ) ),
 .UNSPECIFIED., .T., .F., .F. ) 
 B_SPLINE_SURFACE_WITH_KNOTS ( ( 4, 3, 4 ),
 ( 3, 2, 2, 2, 2, 2, 2, 2, 2, 2, 2, 2, 2, 2, 2, 2, 2, 2, 2, 2, 2, 2, 2, 2, 2, 2, 2, 2, 2, 2, 2, 2, 2, 2, 2, 2, 2, 2, 2, 2, 2, 2, 2, 2, 2, 2, 2, 2, 3 ),
 ( 0.000000000000000000, 0.5000000000000000000, 1.000000000000000000 ),
 ( 0.000000000000000000, 0.02083333333333333218, 0.04166666666666666435, 0.06250000000000000000, 0.08333333333333332871, 0.1041666666666666713, 0.1250000000000000000, 0.1458333333333333426, 0.1666666666666666574, 0.1875000000000000000, 0.2083333333333333426, 0.2291666666666666574, 0.2500000000000000000, 0.2708333333333333148, 0.2916666666666666852, 0.3125000000000000000, 0.3333333333333333148, 0.3541666666666666852, 0.3750000000000000000, 0.3958333333333333148, 0.4166666666666666852, 0.4375000000000000000, 0.4583333333333333148, 0.4791666666666666852, 0.5000000000000000000, 0.5208333333333333703, 0.5416666666666666297, 0.5625000000000000000, 0.5833333333333333703, 0.6041666666666666297, 0.6250000000000000000, 0.6458333333333333703, 0.6666666666666666297, 0.6875000000000000000, 0.7083333333333333703, 0.7291666666666666297, 0.7500000000000000000, 0.7708333333333333703, 0.7916666666666666297, 0.8125000000000000000, 0.8333333333333333703, 0.8541666666666666297, 0.8750000000000000000, 0.8958333333333333703, 0.9166666666666666297, 0.9375000000000000000, 0.9583333333333333703, 0.9791666666666666297, 1.000000000000000000 ),
 .UNSPECIFIED. ) 
 GEOMETRIC_REPRESENTATION_ITEM ( )  RATIONAL_B_SPLINE_SURFACE ( (
 ( 1.000000000000000000, 0.9238795325112867385, 1.000000000000000000, 0.9238795325112867385, 1.000000000000000000, 0.9238795325112867385, 1.000000000000000000, 0.9238795325112867385, 1.000000000000000000, 0.9238795325112867385, 1.000000000000000000, 0.9238795325112867385, 1.000000000000000000, 0.9238795325112867385, 1.000000000000000000, 0.9238795325112867385, 1.000000000000000000, 0.9238795325112867385, 1.000000000000000000, 0.9238795325112867385, 1.000000000000000000, 0.9238795325112867385, 1.000000000000000000, 0.9238795325112867385, 1.000000000000000000, 0.9238795325112867385, 1.000000000000000000, 0.9238795325112867385, 1.000000000000000000, 0.9238795325112867385, 1.000000000000000000, 0.9238795325112867385, 1.000000000000000000, 0.9238795325112867385, 1.000000000000000000, 0.9238795325112867385, 1.000000000000000000, 0.9238795325112867385, 1.000000000000000000, 0.9238795325112867385, 1.000000000000000000, 0.9238795325112867385, 1.000000000000000000, 0.9238795325112867385, 1.000000000000000000, 0.9238795325112867385, 1.000000000000000000, 0.9238795325112867385, 1.000000000000000000, 0.9238795325112867385, 1.000000000000000000, 0.9238795325112867385, 1.000000000000000000, 0.9238795325112867385, 1.000000000000000000, 0.9238795325112867385, 1.000000000000000000, 0.9238795325112867385, 1.000000000000000000, 0.9238795325112867385, 1.000000000000000000, 0.9238795325112867385, 1.000000000000000000, 0.9238795325112867385, 1.000000000000000000, 0.9238795325112867385, 1.000000000000000000, 0.9238795325112867385, 1.000000000000000000, 0.9238795325112867385, 1.000000000000000000, 0.9238795325112867385, 1.000000000000000000, 0.9238795325112867385, 1.000000000000000000, 0.9238795325112867385, 1.000000000000000000, 0.9238795325112867385, 1.000000000000000000, 0.9238795325112867385, 1.000000000000000000, 0.9238795325112867385, 1.000000000000000000, 0.9238795325112867385, 1.000000000000000000, 0.9238795325112867385, 1.000000000000000000, 0.9238795325112867385, 1.000000000000000000, 0.9238795325112867385, 1.000000000000000000, 0.9238795325112867385, 1.000000000000000000, 0.9238795325112867385, 1.000000000000000000, 0.9238795325112867385, 1.000000000000000000),
 ( 0.3333333333333333703, 0.3079598441704289313, 0.3333333333333333703, 0.3079598441704289313, 0.3333333333333333703, 0.3079598441704289313, 0.3333333333333333703, 0.3079598441704289313, 0.3333333333333333703, 0.3079598441704289313, 0.3333333333333333703, 0.3079598441704289313, 0.3333333333333333703, 0.3079598441704289313, 0.3333333333333333703, 0.3079598441704289313, 0.3333333333333333703, 0.3079598441704289313, 0.3333333333333333703, 0.3079598441704289313, 0.3333333333333333703, 0.3079598441704289313, 0.3333333333333333703, 0.3079598441704289313, 0.3333333333333333703, 0.3079598441704289313, 0.3333333333333333703, 0.3079598441704289313, 0.3333333333333333703, 0.3079598441704289313, 0.3333333333333333703, 0.3079598441704289313, 0.3333333333333333703, 0.3079598441704289313, 0.3333333333333333703, 0.3079598441704289313, 0.3333333333333333703, 0.3079598441704289313, 0.3333333333333333703, 0.3079598441704289313, 0.3333333333333333703, 0.3079598441704289313, 0.3333333333333333703, 0.3079598441704289313, 0.3333333333333333703, 0.3079598441704289313, 0.3333333333333333703, 0.3079598441704289313, 0.3333333333333333703, 0.3079598441704289313, 0.3333333333333333703, 0.3079598441704289313, 0.3333333333333333703, 0.3079598441704289313, 0.3333333333333333703, 0.3079598441704289313, 0.3333333333333333703, 0.3079598441704289313, 0.3333333333333333703, 0.3079598441704289313, 0.3333333333333333703, 0.3079598441704289313, 0.3333333333333333703, 0.3079598441704289313, 0.3333333333333333703, 0.3079598441704289313, 0.3333333333333333703, 0.3079598441704289313, 0.3333333333333333703, 0.3079598441704289313, 0.3333333333333333703, 0.3079598441704289313, 0.3333333333333333703, 0.3079598441704289313, 0.3333333333333333703, 0.3079598441704289313, 0.3333333333333333703, 0.3079598441704289313, 0.3333333333333333703, 0.3079598441704289313, 0.3333333333333333703, 0.3079598441704289313, 0.3333333333333333703, 0.3079598441704289313, 0.3333333333333333703, 0.3079598441704289313, 0.3333333333333333703, 0.3079598441704289313, 0.3333333333333333703, 0.3079598441704289313, 0.3333333333333333703, 0.3079598441704289313, 0.3333333333333333703, 0.3079598441704289313, 0.3333333333333333703, 0.3079598441704289313, 0.3333333333333333703),
 ( 0.3333333333333333703, 0.3079598441704289313, 0.3333333333333333703, 0.3079598441704289313, 0.3333333333333333703, 0.3079598441704289313, 0.3333333333333333703, 0.3079598441704289313, 0.3333333333333333703, 0.3079598441704289313, 0.3333333333333333703, 0.3079598441704289313, 0.3333333333333333703, 0.3079598441704289313, 0.3333333333333333703, 0.3079598441704289313, 0.3333333333333333703, 0.3079598441704289313, 0.3333333333333333703, 0.3079598441704289313, 0.3333333333333333703, 0.3079598441704289313, 0.3333333333333333703, 0.3079598441704289313, 0.3333333333333333703, 0.3079598441704289313, 0.3333333333333333703, 0.3079598441704289313, 0.3333333333333333703, 0.3079598441704289313, 0.3333333333333333703, 0.3079598441704289313, 0.3333333333333333703, 0.3079598441704289313, 0.3333333333333333703, 0.3079598441704289313, 0.3333333333333333703, 0.3079598441704289313, 0.3333333333333333703, 0.3079598441704289313, 0.3333333333333333703, 0.3079598441704289313, 0.3333333333333333703, 0.3079598441704289313, 0.3333333333333333703, 0.3079598441704289313, 0.3333333333333333703, 0.3079598441704289313, 0.3333333333333333703, 0.3079598441704289313, 0.3333333333333333703, 0.3079598441704289313, 0.3333333333333333703, 0.3079598441704289313, 0.3333333333333333703, 0.3079598441704289313, 0.3333333333333333703, 0.3079598441704289313, 0.3333333333333333703, 0.3079598441704289313, 0.3333333333333333703, 0.3079598441704289313, 0.3333333333333333703, 0.3079598441704289313, 0.3333333333333333703, 0.3079598441704289313, 0.3333333333333333703, 0.3079598441704289313, 0.3333333333333333703, 0.3079598441704289313, 0.3333333333333333703, 0.3079598441704289313, 0.3333333333333333703, 0.3079598441704289313, 0.3333333333333333703, 0.3079598441704289313, 0.3333333333333333703, 0.3079598441704289313, 0.3333333333333333703, 0.3079598441704289313, 0.3333333333333333703, 0.3079598441704289313, 0.3333333333333333703, 0.3079598441704289313, 0.3333333333333333703, 0.3079598441704289313, 0.3333333333333333703, 0.3079598441704289313, 0.3333333333333333703, 0.3079598441704289313, 0.3333333333333333703, 0.3079598441704289313, 0.3333333333333333703, 0.3079598441704289313, 0.3333333333333333703, 0.3079598441704289313, 0.3333333333333333703),
 ( 1.000000000000000000, 0.9238795325112867385, 1.000000000000000000, 0.9238795325112867385, 1.000000000000000000, 0.9238795325112867385, 1.000000000000000000, 0.9238795325112867385, 1.000000000000000000, 0.9238795325112867385, 1.000000000000000000, 0.9238795325112867385, 1.000000000000000000, 0.9238795325112867385, 1.000000000000000000, 0.9238795325112867385, 1.000000000000000000, 0.9238795325112867385, 1.000000000000000000, 0.9238795325112867385, 1.000000000000000000, 0.9238795325112867385, 1.000000000000000000, 0.9238795325112867385, 1.000000000000000000, 0.9238795325112867385, 1.000000000000000000, 0.9238795325112867385, 1.000000000000000000, 0.9238795325112867385, 1.000000000000000000, 0.9238795325112867385, 1.000000000000000000, 0.9238795325112867385, 1.000000000000000000, 0.9238795325112867385, 1.000000000000000000, 0.9238795325112867385, 1.000000000000000000, 0.9238795325112867385, 1.000000000000000000, 0.9238795325112867385, 1.000000000000000000, 0.9238795325112867385, 1.000000000000000000, 0.9238795325112867385, 1.000000000000000000, 0.9238795325112867385, 1.000000000000000000, 0.9238795325112867385, 1.000000000000000000, 0.9238795325112867385, 1.000000000000000000, 0.9238795325112867385, 1.000000000000000000, 0.9238795325112867385, 1.000000000000000000, 0.9238795325112867385, 1.000000000000000000, 0.9238795325112867385, 1.000000000000000000, 0.9238795325112867385, 1.000000000000000000, 0.9238795325112867385, 1.000000000000000000, 0.9238795325112867385, 1.000000000000000000, 0.9238795325112867385, 1.000000000000000000, 0.9238795325112867385, 1.000000000000000000, 0.9238795325112867385, 1.000000000000000000, 0.9238795325112867385, 1.000000000000000000, 0.9238795325112867385, 1.000000000000000000, 0.9238795325112867385, 1.000000000000000000, 0.9238795325112867385, 1.000000000000000000, 0.9238795325112867385, 1.000000000000000000, 0.9238795325112867385, 1.000000000000000000, 0.9238795325112867385, 1.000000000000000000, 0.9238795325112867385, 1.000000000000000000, 0.9238795325112867385, 1.000000000000000000, 0.9238795325112867385, 1.000000000000000000, 0.9238795325112867385, 1.000000000000000000, 0.9238795325112867385, 1.000000000000000000),
 ( 0.3333333333333333703, 0.3079598441704289313, 0.3333333333333333703, 0.3079598441704289313, 0.3333333333333333703, 0.3079598441704289313, 0.3333333333333333703, 0.3079598441704289313, 0.3333333333333333703, 0.3079598441704289313, 0.3333333333333333703, 0.3079598441704289313, 0.3333333333333333703, 0.3079598441704289313, 0.3333333333333333703, 0.3079598441704289313, 0.3333333333333333703, 0.3079598441704289313, 0.3333333333333333703, 0.3079598441704289313, 0.3333333333333333703, 0.3079598441704289313, 0.3333333333333333703, 0.3079598441704289313, 0.3333333333333333703, 0.3079598441704289313, 0.3333333333333333703, 0.3079598441704289313, 0.3333333333333333703, 0.3079598441704289313, 0.3333333333333333703, 0.3079598441704289313, 0.3333333333333333703, 0.3079598441704289313, 0.3333333333333333703, 0.3079598441704289313, 0.3333333333333333703, 0.3079598441704289313, 0.3333333333333333703, 0.3079598441704289313, 0.3333333333333333703, 0.3079598441704289313, 0.3333333333333333703, 0.3079598441704289313, 0.3333333333333333703, 0.3079598441704289313, 0.3333333333333333703, 0.3079598441704289313, 0.3333333333333333703, 0.3079598441704289313, 0.3333333333333333703, 0.3079598441704289313, 0.3333333333333333703, 0.3079598441704289313, 0.3333333333333333703, 0.3079598441704289313, 0.3333333333333333703, 0.3079598441704289313, 0.3333333333333333703, 0.3079598441704289313, 0.3333333333333333703, 0.3079598441704289313, 0.3333333333333333703, 0.3079598441704289313, 0.3333333333333333703, 0.3079598441704289313, 0.3333333333333333703, 0.3079598441704289313, 0.3333333333333333703, 0.3079598441704289313, 0.3333333333333333703, 0.3079598441704289313, 0.3333333333333333703, 0.3079598441704289313, 0.3333333333333333703, 0.3079598441704289313, 0.3333333333333333703, 0.3079598441704289313, 0.3333333333333333703, 0.3079598441704289313, 0.3333333333333333703, 0.3079598441704289313, 0.3333333333333333703, 0.3079598441704289313, 0.3333333333333333703, 0.3079598441704289313, 0.3333333333333333703, 0.3079598441704289313, 0.3333333333333333703, 0.3079598441704289313, 0.3333333333333333703, 0.3079598441704289313, 0.3333333333333333703, 0.3079598441704289313, 0.3333333333333333703, 0.3079598441704289313, 0.3333333333333333703),
 ( 0.3333333333333333703, 0.3079598441704289313, 0.3333333333333333703, 0.3079598441704289313, 0.3333333333333333703, 0.3079598441704289313, 0.3333333333333333703, 0.3079598441704289313, 0.3333333333333333703, 0.3079598441704289313, 0.3333333333333333703, 0.3079598441704289313, 0.3333333333333333703, 0.3079598441704289313, 0.3333333333333333703, 0.3079598441704289313, 0.3333333333333333703, 0.3079598441704289313, 0.3333333333333333703, 0.3079598441704289313, 0.3333333333333333703, 0.3079598441704289313, 0.3333333333333333703, 0.3079598441704289313, 0.3333333333333333703, 0.3079598441704289313, 0.3333333333333333703, 0.3079598441704289313, 0.3333333333333333703, 0.3079598441704289313, 0.3333333333333333703, 0.3079598441704289313, 0.3333333333333333703, 0.3079598441704289313, 0.3333333333333333703, 0.3079598441704289313, 0.3333333333333333703, 0.3079598441704289313, 0.3333333333333333703, 0.3079598441704289313, 0.3333333333333333703, 0.3079598441704289313, 0.3333333333333333703, 0.3079598441704289313, 0.3333333333333333703, 0.3079598441704289313, 0.3333333333333333703, 0.3079598441704289313, 0.3333333333333333703, 0.3079598441704289313, 0.3333333333333333703, 0.3079598441704289313, 0.3333333333333333703, 0.3079598441704289313, 0.3333333333333333703, 0.3079598441704289313, 0.3333333333333333703, 0.3079598441704289313, 0.3333333333333333703, 0.3079598441704289313, 0.3333333333333333703, 0.3079598441704289313, 0.3333333333333333703, 0.3079598441704289313, 0.3333333333333333703, 0.3079598441704289313, 0.3333333333333333703, 0.3079598441704289313, 0.3333333333333333703, 0.3079598441704289313, 0.3333333333333333703, 0.3079598441704289313, 0.3333333333333333703, 0.3079598441704289313, 0.3333333333333333703, 0.3079598441704289313, 0.3333333333333333703, 0.3079598441704289313, 0.3333333333333333703, 0.3079598441704289313, 0.3333333333333333703, 0.3079598441704289313, 0.3333333333333333703, 0.3079598441704289313, 0.3333333333333333703, 0.3079598441704289313, 0.3333333333333333703, 0.3079598441704289313, 0.3333333333333333703, 0.3079598441704289313, 0.3333333333333333703, 0.3079598441704289313, 0.3333333333333333703, 0.3079598441704289313, 0.3333333333333333703, 0.3079598441704289313, 0.3333333333333333703),
 ( 1.000000000000000000, 0.9238795325112867385, 1.000000000000000000, 0.9238795325112867385, 1.000000000000000000, 0.9238795325112867385, 1.000000000000000000, 0.9238795325112867385, 1.000000000000000000, 0.9238795325112867385, 1.000000000000000000, 0.9238795325112867385, 1.000000000000000000, 0.9238795325112867385, 1.000000000000000000, 0.9238795325112867385, 1.000000000000000000, 0.9238795325112867385, 1.000000000000000000, 0.9238795325112867385, 1.000000000000000000, 0.9238795325112867385, 1.000000000000000000, 0.9238795325112867385, 1.000000000000000000, 0.9238795325112867385, 1.000000000000000000, 0.9238795325112867385, 1.000000000000000000, 0.9238795325112867385, 1.000000000000000000, 0.9238795325112867385, 1.000000000000000000, 0.9238795325112867385, 1.000000000000000000, 0.9238795325112867385, 1.000000000000000000, 0.9238795325112867385, 1.000000000000000000, 0.9238795325112867385, 1.000000000000000000, 0.9238795325112867385, 1.000000000000000000, 0.9238795325112867385, 1.000000000000000000, 0.9238795325112867385, 1.000000000000000000, 0.9238795325112867385, 1.000000000000000000, 0.9238795325112867385, 1.000000000000000000, 0.9238795325112867385, 1.000000000000000000, 0.9238795325112867385, 1.000000000000000000, 0.9238795325112867385, 1.000000000000000000, 0.9238795325112867385, 1.000000000000000000, 0.9238795325112867385, 1.000000000000000000, 0.9238795325112867385, 1.000000000000000000, 0.9238795325112867385, 1.000000000000000000, 0.9238795325112867385, 1.000000000000000000, 0.9238795325112867385, 1.000000000000000000, 0.9238795325112867385, 1.000000000000000000, 0.9238795325112867385, 1.000000000000000000, 0.9238795325112867385, 1.000000000000000000, 0.9238795325112867385, 1.000000000000000000, 0.9238795325112867385, 1.000000000000000000, 0.9238795325112867385, 1.000000000000000000, 0.9238795325112867385, 1.000000000000000000, 0.9238795325112867385, 1.000000000000000000, 0.9238795325112867385, 1.000000000000000000, 0.9238795325112867385, 1.000000000000000000, 0.9238795325112867385, 1.000000000000000000, 0.9238795325112867385, 1.000000000000000000, 0.9238795325112867385, 1.000000000000000000, 0.9238795325112867385, 1.000000000000000000) ) ) 
 REPRESENTATION_ITEM ( '' )  SURFACE ( )  );
#16497 = CARTESIAN_POINT ( 'NONE',  ( 13.50000000000000000, 60.42999999999999972, 1.653273178848926867E-15 ) ) ;
#16498 = CARTESIAN_POINT ( 'NONE',  ( 13.50000000000000000, 50.42999999999999972, 1.653273178848926867E-15 ) ) ;
#16499 = CARTESIAN_POINT ( 'NONE',  ( -12.41413396520435874, 53.12371177561935554, 5.309278927454689878 ) ) ;
#16500 = CARTESIAN_POINT ( 'NONE',  ( -11.76794919243112325, 39.07999999999999119, 3.823638476888994386 ) ) ;
#16501 = CARTESIAN_POINT ( 'NONE',  ( 9.520470885617715595, -18.86999999999999744, 6.917026985038135400 ) ) ;
#16502 = CARTESIAN_POINT ( 'NONE',  ( -10.92172942406178926, 60.63000000000000256, -7.935100905948389460 ) ) ;
#16503 = CYLINDRICAL_SURFACE ( 'NONE', #528, 12.00000000000000178 ) ;
#16504 = CARTESIAN_POINT ( 'NONE',  ( 6.513726533578187983, 68.91946989124797085, 11.83231862531209444 ) ) ;
#16505 = CARTESIAN_POINT ( 'NONE',  ( -3.394498949081906414, 37.30204389133518106, -13.06947235405735519 ) ) ;
#16506 = CARTESIAN_POINT ( 'NONE',  ( -8.291044507619272909E-14, 57.17999999999999972, -13.50000000000000000 ) ) ;
#16507 = CARTESIAN_POINT ( 'NONE',  ( -1.564113515457998370E-12, -86.33749999999982094, 18.62500000000000000 ) ) ;
#16508 = CARTESIAN_POINT ( 'NONE',  ( -10.67600666061439973, 74.24413227333732834, 8.265984108055215884 ) ) ;
#16509 = CARTESIAN_POINT ( 'NONE',  ( -4.628240636438917477, 76.34660530185777816, -12.68187234864826607 ) ) ;
#16510 = CARTESIAN_POINT ( 'NONE',  ( -1.059413705080190837, 79.21809260812437969, -13.49999987874332241 ) ) ;
#16511 = DIRECTION ( 'NONE',  ( -0.000000000000000000, -1.000000000000000000, -0.000000000000000000 ) ) ;
#16512 = CYLINDRICAL_SURFACE ( 'NONE', #15012, 1.999999999999998224 ) ;
#16513 = CARTESIAN_POINT ( 'NONE',  ( 2.621994543952811015E-15, 32.18000000000000682, -14.19474002721660355 ) ) ;
#16514 = CARTESIAN_POINT ( 'NONE',  ( 3.636496289402157078, -5.969999999999996199, -11.19198476289190936 ) ) ;
#16515 = CARTESIAN_POINT ( 'NONE',  ( 7.272992578804311492, 40.87999999999999545, -10.01041549318726886 ) ) ;
#16516 = CARTESIAN_POINT ( 'NONE',  ( 2.445080149700053643E-15, 1.180000000000002602, -13.50000000000000000 ) ) ;
#16517 = EDGE_CURVE ( 'NONE', #11619, #7799, #10881, .T. ) ;
#16518 = CARTESIAN_POINT ( 'NONE',  ( -9.459099616640498809, 32.30840304435178467, 9.632024434120667777 ) ) ;
#16519 = CARTESIAN_POINT ( 'NONE',  ( 13.07675211750358457, 75.54939648288200260, -3.353959690592315912 ) ) ;
#16520 = CARTESIAN_POINT ( 'NONE',  ( 3.329803442097187371, -7.135244913870566388E-13, -15.09609079982930524 ) ) ;
#16521 = CARTESIAN_POINT ( 'NONE',  ( 7.272992578804311492, 31.87999999999999545, -10.01041549318726709 ) ) ;
#16522 = CARTESIAN_POINT ( 'NONE',  ( -4.171729424061787483, 81.32999999999999829, -12.83926296998457417 ) ) ;
#16523 = CARTESIAN_POINT ( 'NONE',  ( 7.855212290319397717, 51.88356205845266800, -10.98026488807781931 ) ) ;
#16524 = CIRCLE ( 'NONE', #3253, 5.000000000000000000 ) ;
#16525 = CARTESIAN_POINT ( 'NONE',  ( -1.457356408888724308, 38.62762465094729691, 13.42125827019123463 ) ) ;
#16526 = CARTESIAN_POINT ( 'NONE',  ( 3.493089250578063520, 37.05461647915249301, -13.07001197377214119 ) ) ;
#16527 = LINE ( 'NONE', #1413, #2587 ) ;
#16528 = PLANE ( 'NONE',  #12614 ) ;
#16529 = CARTESIAN_POINT ( 'NONE',  ( 7.235470476593615530, 62.94958575296288927, 11.39775609064293427 ) ) ;
#16530 = CARTESIAN_POINT ( 'NONE',  ( 13.50300513245434431, 42.42850705580203652, 0.04008974157810932942 ) ) ;
#16531 = CARTESIAN_POINT ( 'NONE',  ( 7.173772269966901760, 48.91298932173004488, -11.43911279990962448 ) ) ;
#16532 = CARTESIAN_POINT ( 'NONE',  ( 9.520470885617717371, 23.73000000000000043, -6.917026985038131848 ) ) ;
#16533 = EDGE_LOOP ( 'NONE', ( #14479, #9698, #17464, #5606 ) ) ;
#16534 = CARTESIAN_POINT ( 'NONE',  ( 9.520470885617717371, 67.73000000000000398, -6.917026985038131848 ) ) ;
#16535 = CARTESIAN_POINT ( 'NONE',  ( -3.943571451878268075, 70.32179627606707584, -12.91117844506843859 ) ) ;
#16536 = CARTESIAN_POINT ( 'NONE',  ( -8.043339635996302306, -22.89374999999994387, -8.043339635997654113 ) ) ;
#16537 = CARTESIAN_POINT ( 'NONE',  ( -13.49999999999999822, 10.77999999999999936, -4.386415899144240349 ) ) ;
#16538 = VERTEX_POINT ( 'NONE', #3234 ) ;
#16539 = CARTESIAN_POINT ( 'NONE',  ( -11.11731508959757342, 43.64162586097864960, -7.658681678614005506 ) ) ;
#16540 = CARTESIAN_POINT ( 'NONE',  ( 6.123233995736766282E-16, 3.000000000000000000, 5.000000000000000000 ) ) ;
#16541 = CARTESIAN_POINT ( 'NONE',  ( 13.49453415536198797, 60.44356499961826046, -0.3946668185908841497 ) ) ;
#16542 = CIRCLE ( 'NONE', #11195, 3.624999999999999556 ) ;
#16543 = CARTESIAN_POINT ( 'NONE',  ( 4.171729424061789260, 3.830000000000000071, 12.83926296998457239 ) ) ;
#16544 = DIRECTION ( 'NONE',  ( -0.000000000000000000, 1.000000000000000000, -0.000000000000000000 ) ) ;
#16545 = CARTESIAN_POINT ( 'NONE',  ( 12.92234882186717115, 66.28998143173690494, 3.906840215585264176 ) ) ;
#16546 = CARTESIAN_POINT ( 'NONE',  ( 10.65812523510989607, 57.11492007506318203, 8.285798828776941960 ) ) ;
#16547 = CARTESIAN_POINT ( 'NONE',  ( 7.272992578804308828, 60.97999999999999687, 10.01041549318726709 ) ) ;
#16548 = CARTESIAN_POINT ( 'NONE',  ( -9.520470885617715595, 68.62999999999999545, -6.917026985038136289 ) ) ;
#16549 = CARTESIAN_POINT ( 'NONE',  ( -12.55849098233041516, 46.75015478663139845, -4.953260354883232353 ) ) ;
#16550 = CARTESIAN_POINT ( 'NONE',  ( 7.207449306385443677, 45.91159972359503172, -11.41531860434902512 ) ) ;
#16551 = CARTESIAN_POINT ( 'NONE',  ( 1.900613283887800264, 9.237093173895598142, -12.00000000000222045 ) ) ;
#16552 = CARTESIAN_POINT ( 'NONE',  ( -23.28534784291395709, 6.548267719634617734, -4.206197538246709833 ) ) ;
#16553 = CARTESIAN_POINT ( 'NONE',  ( 5.020134451633054162, 30.99833425099403428, -12.53726460365605710 ) ) ;
#16554 = CARTESIAN_POINT ( 'NONE',  ( -6.237188668602095198, 56.45156311056310017, 11.97644378720688785 ) ) ;
#16555 = CARTESIAN_POINT ( 'NONE',  ( 11.37499999999960210, -98.85937499999975842, 4.711679271994918317 ) ) ;
#16556 = AXIS2_PLACEMENT_3D ( 'NONE', #14609, #17094, #9169 ) ;
#16557 = CYLINDRICAL_SURFACE ( 'NONE', #15405, 13.50000000000000000 ) ;
#16558 = CARTESIAN_POINT ( 'NONE',  ( 4.772672689868944218, 32.85189186562215014, 12.63022836692152495 ) ) ;
#16559 = CARTESIAN_POINT ( 'NONE',  ( 15.58845726811991916, 0.000000000000000000, -10.99999999999996092 ) ) ;
#16560 = CARTESIAN_POINT ( 'NONE',  ( 4.352287195575301304, 40.02347799479684198, -12.77918881344716517 ) ) ;
#16561 = VERTEX_POINT ( 'NONE', #8654 ) ;
#16562 = CARTESIAN_POINT ( 'NONE',  ( -8.673344535932200117, 62.34634085401044956, 10.34522302012570449 ) ) ;
#16563 = ORIENTED_EDGE ( 'NONE', *, *, #13127, .F. ) ;
#16564 = CARTESIAN_POINT ( 'NONE',  ( -13.37780778470979648, 40.99393780181782887, 1.830007199971625420 ) ) ;
#16565 = CARTESIAN_POINT ( 'NONE',  ( -3.636496289402156190, -13.46999999999999531, 11.19198476289190758 ) ) ;
#16566 = CARTESIAN_POINT ( 'NONE',  ( 1.561832610794586740E-12, -44.71249999999991331, -18.62500000000000000 ) ) ;
#16567 = CARTESIAN_POINT ( 'NONE',  ( -12.88197876152688615, 43.78491403648499158, -4.041588179776032241 ) ) ;
#16568 = CARTESIAN_POINT ( 'NONE',  ( 13.50000000000000000, 0.4300000000000137046, 1.734723475976807094E-15 ) ) ;
#16569 = CARTESIAN_POINT ( 'NONE',  ( -8.343458848123582072, 35.37999999999999545, 11.48378591275254124 ) ) ;
#16570 = CARTESIAN_POINT ( 'NONE',  ( -8.343458848123576743, 48.48000000000000398, -11.48378591275254301 ) ) ;
#16571 = CARTESIAN_POINT ( 'NONE',  ( -0.009212933485843630491, 46.18033114546576456, -13.49999764172323147 ) ) ;
#16572 = ADVANCED_FACE ( 'NONE', ( #7319 ), #590, .T. ) ;
#16573 = CARTESIAN_POINT ( 'NONE',  ( -5.559764996625593092, 67.38173173404518934, -12.30199985033388010 ) ) ;
#16574 = CARTESIAN_POINT ( 'NONE',  ( -7.714727599200466912, -70.79687499999981526, 18.62499999999935341 ) ) ;
#16575 = CARTESIAN_POINT ( 'NONE',  ( 6.586770268181092014, 53.92254834050746126, 11.78407759566256985 ) ) ;
#16576 = CARTESIAN_POINT ( 'NONE',  ( -3.270141562520593403, 64.29757460427565263, -13.09794721236131210 ) ) ;
#16577 = EDGE_LOOP ( 'NONE', ( #583, #11115, #10636, #8016 ) ) ;
#16578 = CARTESIAN_POINT ( 'NONE',  ( -10.20076248856652867, 34.58984148594135632, -8.842762936844939858 ) ) ;
#16579 = CARTESIAN_POINT ( 'NONE',  ( -9.552639591052204498E-13, -29.13749999999993179, 11.37500000000000000 ) ) ;
#16580 = CARTESIAN_POINT ( 'NONE',  ( 12.85115454411534053, 78.28138835478902990, 4.134994248532485095 ) ) ;
#16581 = CARTESIAN_POINT ( 'NONE',  ( -15.43183772185609826, 8.055054230040788354, 9.319033143234966232 ) ) ;
#16582 = CARTESIAN_POINT ( 'NONE',  ( 7.500000000000000000, -24.01085892585522430, -8.949127168380909936 ) ) ;
#16583 = CARTESIAN_POINT ( 'NONE',  ( 13.37012903279583576, 72.36469939934085005, 1.868140815954207001 ) ) ;
#16584 = CARTESIAN_POINT ( 'NONE',  ( -8.549982208541774191E-16, -14.32000000000000561, 14.19474002721660355 ) ) ;
#16585 = CARTESIAN_POINT ( 'NONE',  ( 8.343458848123583849, 63.87999999999998835, -11.48378591275253768 ) ) ;
#16586 = CARTESIAN_POINT ( 'NONE',  ( -0.7864078588604943576, 71.65172976531886206, 13.47770389585425832 ) ) ;
#16587 = CARTESIAN_POINT ( 'NONE',  ( 2.272985001014427788E-15, 35.17999999999998550, -12.37355403259654985 ) ) ;
#16588 = CARTESIAN_POINT ( 'NONE',  ( -10.92172942406179104, 58.23000000000000398, 7.935100905948387684 ) ) ;
#16589 = DIRECTION ( 'NONE',  ( -0.000000000000000000, -1.000000000000000000, -0.000000000000000000 ) ) ;
#16590 = CARTESIAN_POINT ( 'NONE',  ( 9.520470885617717371, -3.269999999999995133, -6.917026985038131848 ) ) ;
#16591 = CARTESIAN_POINT ( 'NONE',  ( 11.35791665574828713, 69.15656779720782765, 7.300441548434104533 ) ) ;
#16592 = CARTESIAN_POINT ( 'NONE',  ( -2.862087262652846853, 37.28290999384705628, -13.19312863063275998 ) ) ;
#16593 = ADVANCED_FACE ( 'NONE', ( #2159 ), #12877, .T. ) ;
#16594 = CARTESIAN_POINT ( 'NONE',  ( 7.416407864998737054, 4.846025403784445018, 10.20780970022447853 ) ) ;
#16595 = CARTESIAN_POINT ( 'NONE',  ( -7.714727599197334307, -95.70312499999980105, -18.62500000000064659 ) ) ;
#16596 = CARTESIAN_POINT ( 'NONE',  ( -11.40798122654512525, 73.65990416871910895, -7.218615817919470601 ) ) ;
#16597 = CARTESIAN_POINT ( 'NONE',  ( -6.942184294231981134, 76.43724017907349833, -11.57843550520342113 ) ) ;
#16598 = CARTESIAN_POINT ( 'NONE',  ( -4.363074663832638755, 79.33691353306146254, -12.77551180107495199 ) ) ;
#16599 = CARTESIAN_POINT ( 'NONE',  ( -12.00000000000000178, 0.9460254037844377795, 3.899036354794875869 ) ) ;
#16600 = DIRECTION ( 'NONE',  ( 0.000000000000000000, 0.000000000000000000, -1.000000000000000000 ) ) ;
#16601 = CARTESIAN_POINT ( 'NONE',  ( 4.171729424061791924, 32.03000000000000114, -12.83926296998457239 ) ) ;
#16602 = CARTESIAN_POINT ( 'NONE',  ( -11.76794919243112325, -10.92000000000000526, 3.823638476888994386 ) ) ;
#16603 = CARTESIAN_POINT ( 'NONE',  ( -7.272992578804310604, 36.37999999999998835, 10.01041549318726886 ) ) ;
#16604 =( BOUNDED_CURVE ( )  B_SPLINE_CURVE ( 2, ( #2975, #4501, #8905, #17007, #9908, #15255, #8405, #1746, #4824, #515, #16417, #12543, #1657 ),
 .UNSPECIFIED., .F., .F. ) 
 B_SPLINE_CURVE_WITH_KNOTS ( ( 3, 2, 2, 2, 2, 2, 3 ),
 ( 0.2083333333333333148, 0.2111111111111111105, 0.2166666666666666741, 0.2222222222222222099, 0.2277777777777777735, 0.2333333333333333370, 0.2361111111111111049 ),
 .UNSPECIFIED. ) 
 CURVE ( )  GEOMETRIC_REPRESENTATION_ITEM ( )  RATIONAL_B_SPLINE_CURVE ( ( 0.9755282581475765991, 0.9755282581475765991, 1.000000000000000000, 0.9510565162951535312, 1.000000000000000000, 0.9510565162951535312, 1.000000000000000000, 0.9510565162951535312, 1.000000000000000000, 0.9510565162951535312, 1.000000000000000000, 0.9755282581475768211, 0.9755282581475765991 ) ) 
 REPRESENTATION_ITEM ( '' )  );
#16605 = CARTESIAN_POINT ( 'NONE',  ( 2.621994543952811015E-15, -13.82000000000000028, -14.19474002721660355 ) ) ;
#16606 = CARTESIAN_POINT ( 'NONE',  ( -7.096040157522595315, 32.41630410450128608, 11.48461955335362106 ) ) ;
#16607 = CARTESIAN_POINT ( 'NONE',  ( 2.717229725162839227, 74.77768976466231265, 13.22563761779151825 ) ) ;
#16608 = CARTESIAN_POINT ( 'NONE',  ( 11.21760822425125603, -2.318222727469663182E-13, -13.78532672430268491 ) ) ;
#16609 = VECTOR ( 'NONE', #1434, 1000.000000000000000 ) ;
#16610 = CARTESIAN_POINT ( 'NONE',  ( -9.520470885617717371, 33.22999999999999687, 6.917026985038133624 ) ) ;
#16611 = CARTESIAN_POINT ( 'NONE',  ( -8.343458848123582072, 82.38000000000000966, 11.48378591275254124 ) ) ;
#16612 = CARTESIAN_POINT ( 'NONE',  ( -2.175153866734307329, 58.25820765909811882, -13.32388992672253636 ) ) ;
#16613 = DIRECTION ( 'NONE',  ( -0.000000000000000000, 1.000000000000000000, -0.000000000000000000 ) ) ;
#16614 = ADVANCED_FACE ( 'NONE', ( #15505, #4924 ), #4835, .T. ) ;
#16615 = CARTESIAN_POINT ( 'NONE',  ( 0.000000000000000000, -1.200000000000000030E-05, 5.000000000000000000 ) ) ;
#16616 = CARTESIAN_POINT ( 'NONE',  ( 17.32050807568878170, 0.000000000000000000, -7.999999999999961808 ) ) ;
#16617 = FACE_OUTER_BOUND ( 'NONE', #10213, .T. ) ;
#16618 = CARTESIAN_POINT ( 'NONE',  ( 5.623418083639327492, 62.88408628963233582, 12.28088165123665654 ) ) ;
#16619 = CARTESIAN_POINT ( 'NONE',  ( 13.35664415350134426, 42.36122446370394101, 1.964704937003258767 ) ) ;
#16620 = CARTESIAN_POINT ( 'NONE',  ( 8.226923464784990259, 48.86690000741498352, -10.70406459611412053 ) ) ;
#16621 = CIRCLE ( 'NONE', #1654, 12.00000000000000178 ) ;
#16622 = CARTESIAN_POINT ( 'NONE',  ( -11.76794919243112325, 25.08000000000001251, 3.823638476888994386 ) ) ;
#16623 = ORIENTED_EDGE ( 'NONE', *, *, #2426, .F. ) ;
#16624 = CARTESIAN_POINT ( 'NONE',  ( -11.76794919243112325, 66.07999999999999829, 3.823638476888994830 ) ) ;
#16625 = CARTESIAN_POINT ( 'NONE',  ( -13.16986379960055409, -86.40624999999977263, 13.16986379959834252 ) ) ;
#16626 = CARTESIAN_POINT ( 'NONE',  ( 4.711679271993006068, -80.12812499999981242, 11.37500000000039257 ) ) ;
#16627 = CARTESIAN_POINT ( 'NONE',  ( 13.49999999999999822, 9.280000000000002913, 4.386415899144237684 ) ) ;
#16628 = VERTEX_POINT ( 'NONE', #7583 ) ;
#16629 = CARTESIAN_POINT ( 'NONE',  ( -0.03816919975528386411, 43.18137242233956385, -13.49994894151539526 ) ) ;
#16630 = CARTESIAN_POINT ( 'NONE',  ( -7.499999999999998224, 107.9345255869305760, 5.560661329642320183 ) ) ;
#16631 = CARTESIAN_POINT ( 'NONE',  ( 13.49999999999999822, 4.280000000000002025, 4.386415899144237684 ) ) ;
#16632 = CARTESIAN_POINT ( 'NONE',  ( -3.708203932499370303, 7.396025403784446617, 11.41267819554184371 ) ) ;
#16633 = CARTESIAN_POINT ( 'NONE',  ( 12.86384301462254420, 66.28284470376391369, 4.096554117506745918 ) ) ;
#16634 = CARTESIAN_POINT ( 'NONE',  ( 10.55353346449092911, 57.10905816187499795, 8.419028628576304740 ) ) ;
#16635 = CARTESIAN_POINT ( 'NONE',  ( -11.76794919243112325, 56.77999999999998693, -3.823638476888998827 ) ) ;
#16636 = CARTESIAN_POINT ( 'NONE',  ( -9.520470885617715595, 71.62999999999999545, -6.917026985038136289 ) ) ;
#16637 = CARTESIAN_POINT ( 'NONE',  ( -13.44822379438176441, 46.88685179129658565, -1.238907302481064843 ) ) ;
#16638 = VECTOR ( 'NONE', #2102, 1000.000000000000000 ) ;
#16639 = CARTESIAN_POINT ( 'NONE',  ( 9.190911557378541374, 45.82162825536664741, -9.888297778096264423 ) ) ;
#16640 = CARTESIAN_POINT ( 'NONE',  ( 5.641748383016213175, 69.97509866883848417, -12.26461152474380256 ) ) ;
#16641 = CARTESIAN_POINT ( 'NONE',  ( 5.850237716920893227, 30.96695511545072321, -12.16654113314289809 ) ) ;
#16642 = CARTESIAN_POINT ( 'NONE',  ( -13.47731147386839012, 55.90299908574060339, -0.7823863207999742775 ) ) ;
#16643 = CARTESIAN_POINT ( 'NONE',  ( 13.50000000000000000, 53.43000000000000682, 1.653273178848926867E-15 ) ) ;
#16644 = CARTESIAN_POINT ( 'NONE',  ( 1.222065048496696615, 32.72394127083357773, 13.44460228257956835 ) ) ;
#16645 = LINE ( 'NONE', #393, #17284 ) ;
#16646 = CARTESIAN_POINT ( 'NONE',  ( 8.221241430366118763, 39.86716037471302343, -10.70805348710604576 ) ) ;
#16647 = ORIENTED_EDGE ( 'NONE', *, *, #12520, .F. ) ;
#16648 = CARTESIAN_POINT ( 'NONE',  ( -12.70043917417899770, 62.09540525535791033, 4.577124250142029283 ) ) ;
#16649 = CARTESIAN_POINT ( 'NONE',  ( -18.62500000000000000, -15.57499999999998153, -1.562973063126292757E-12 ) ) ;
#16650 = CARTESIAN_POINT ( 'NONE',  ( 10.14067890081039636, 48.08657762055307217, 8.914487275897856833 ) ) ;
#16651 = CARTESIAN_POINT ( 'NONE',  ( -9.656730951920790673, 8.027996330223285071, 15.34225977864766932 ) ) ;
#16652 = EDGE_CURVE ( 'NONE', #15567, #13217, #11388, .T. ) ;
#16653 = CARTESIAN_POINT ( 'NONE',  ( 4.171729424061789260, 38.82999999999999829, 12.83926296998457417 ) ) ;
#16654 = AXIS2_PLACEMENT_3D ( 'NONE', #186, #4335, #13945 ) ;
#16655 = CARTESIAN_POINT ( 'NONE',  ( -0.1772876194880645961, 8.062177826491099708, 17.99999999999998934 ) ) ;
#16656 = CARTESIAN_POINT ( 'NONE',  ( -2.956505443956637169, 67.28629095795685089, -13.17228614719877555 ) ) ;
#16657 = CARTESIAN_POINT ( 'NONE',  ( -1.564113515457998370E-12, -55.18749999999985079, 18.62500000000000000 ) ) ;
#16658 = CARTESIAN_POINT ( 'NONE',  ( 6.608087321929540181, 53.92343117755994797, 11.77214407716479450 ) ) ;
#16659 = VERTEX_POINT ( 'NONE', #14356 ) ;
#16660 = CARTESIAN_POINT ( 'NONE',  ( -8.697098998243532012E-15, 64.18000000000002103, -13.50000000000000000 ) ) ;
#16661 = ORIENTED_EDGE ( 'NONE', *, *, #12837, .F. ) ;
#16662 = CARTESIAN_POINT ( 'NONE',  ( 4.171729424061789260, 8.830000000000005400, 12.83926296998457239 ) ) ;
#16663 = CARTESIAN_POINT ( 'NONE',  ( -11.80087666258112122, 34.68689685915391152, -6.556923290561053719 ) ) ;
#16664 = CARTESIAN_POINT ( 'NONE',  ( -13.50000000000000000, 17.92999999999999972, -3.469446951953614189E-15 ) ) ;
#16665 = CARTESIAN_POINT ( 'NONE',  ( 9.538709233711902776E-13, -70.76249999999983231, -11.37500000000000000 ) ) ;
#16666 = CARTESIAN_POINT ( 'NONE',  ( 13.05929335850220419, 78.55189450621524827, -3.421339340133226159 ) ) ;
#16667 = CARTESIAN_POINT ( 'NONE',  ( 1.653273178848926472E-15, 80.93000000000000682, 13.50000000000000000 ) ) ;
#16668 = CARTESIAN_POINT ( 'NONE',  ( 0.000000000000000000, 9.000000000000000000, 0.000000000000000000 ) ) ;
#16669 = CARTESIAN_POINT ( 'NONE',  ( 7.500000000000001776, -26.56718630404941806, 6.484415072061724850 ) ) ;
#16670 = CARTESIAN_POINT ( 'NONE',  ( 13.21136977642124499, 72.52851845461269420, -2.785417675787339231 ) ) ;
#16671 = ADVANCED_FACE ( 'NONE', ( #3585 ), #14272, .T. ) ;
#16672 = CARTESIAN_POINT ( 'NONE',  ( 7.272992578804311492, 29.88000000000000966, -10.01041549318726709 ) ) ;
#16673 = CARTESIAN_POINT ( 'NONE',  ( -10.92172942406178926, 67.62999999999999545, -7.935100905948389460 ) ) ;
#16674 = CARTESIAN_POINT ( 'NONE',  ( -5.802784399048038999, 52.39118405824265778, -12.18924498636963349 ) ) ;
#16675 = CARTESIAN_POINT ( 'NONE',  ( -7.272992578804310604, 39.38000000000000256, 10.01041549318726709 ) ) ;
#16676 = CARTESIAN_POINT ( 'NONE',  ( 13.49999999999999822, 62.28000000000000114, 4.386415899144237684 ) ) ;
#16677 = CARTESIAN_POINT ( 'NONE',  ( -15.58845726811976995, 7.773118517290098062, -11.00000000000018119 ) ) ;
#16678 = CARTESIAN_POINT ( 'NONE',  ( -7.409984580736203970E-16, -4.320000000000003837, 12.37355403259654985 ) ) ;
#16679 = CARTESIAN_POINT ( 'NONE',  ( 4.028353631777413568, 68.82466814077726269, 12.88820194039942990 ) ) ;
#16680 = CARTESIAN_POINT ( 'NONE',  ( 7.714727599200458030, -3.121874999999992628, -18.62499999999934985 ) ) ;
#16681 = DIRECTION ( 'NONE',  ( 0.000000000000000000, -1.000000000000000000, 0.000000000000000000 ) ) ;
#16682 = CARTESIAN_POINT ( 'NONE',  ( 18.62500000000064659, -58.24062499999988063, -7.714727599197336083 ) ) ;
#16683 = CARTESIAN_POINT ( 'NONE',  ( -11.37058303215777499, 73.65747949932976724, -7.277363885997346848 ) ) ;
#16684 = CARTESIAN_POINT ( 'NONE',  ( -9.423580237977008167, 76.54982212202980918, -9.666754949485444115 ) ) ;
#16685 = CARTESIAN_POINT ( 'NONE',  ( -4.194230612231265809, 79.33078485373877697, -12.83233939078419716 ) ) ;
#16686 = CARTESIAN_POINT ( 'NONE',  ( 8.012470509808036212, 7.834275465301278274, -17.06309263661789544 ) ) ;
#16687 = DIRECTION ( 'NONE',  ( 0.000000000000000000, 0.000000000000000000, 1.000000000000000000 ) ) ;
#16688 = CARTESIAN_POINT ( 'NONE',  ( 3.636496289402157078, -2.970000000000000639, -11.19198476289190936 ) ) ;
#16689 = CARTESIAN_POINT ( 'NONE',  ( -7.576616670048093940E-16, 39.67999999999999261, 12.37355403259654807 ) ) ;
#16690 = UNCERTAINTY_MEASURE_WITH_UNIT (LENGTH_MEASURE( 1.000000000000000082E-05 ), #13772, 'distance_accuracy_value', 'NONE');
#16691 = CARTESIAN_POINT ( 'NONE',  ( 12.00000000000000178, 5.413974596215561874, 3.899036354794877202 ) ) ;
#16692 = CARTESIAN_POINT ( 'NONE',  ( -4.511025009967577049, 32.51769489362273902, 12.72403845838506520 ) ) ;
#16693 = CARTESIAN_POINT ( 'NONE',  ( 3.620391450164611058, 74.81017573312026059, 13.00552749220717352 ) ) ;
#16694 = EDGE_CURVE ( 'NONE', #5339, #14160, #13625, .T. ) ;
#16695 = CARTESIAN_POINT ( 'NONE',  ( 10.92172942406179104, 3.730000000000011084, -7.935100905948385908 ) ) ;
#16696 = AXIS2_PLACEMENT_3D ( 'NONE', #8349, #13705, #16451 ) ;
#16697 = DIRECTION ( 'NONE',  ( 0.6531459162717628830, 0.000000000000000000, -0.7572320727871473256 ) ) ;
#16698 = CARTESIAN_POINT ( 'NONE',  ( -8.691771469529815392E-16, 82.67999999999999261, 14.19474002721660355 ) ) ;
#16699 = CARTESIAN_POINT ( 'NONE',  ( 10.03398847469492239, 51.77899704666725711, -9.031564513890813828 ) ) ;
#16700 = CARTESIAN_POINT ( 'NONE',  ( -4.430225406486345996, 38.52064587386139749, 12.75245493685339504 ) ) ;
#16701 = CARTESIAN_POINT ( 'NONE',  ( 4.340749435625693486, 37.02381347075288431, -12.81346088498517233 ) ) ;
#16702 = CARTESIAN_POINT ( 'NONE',  ( 3.785595641572113985E-06, 49.17999986388394973, -13.49999999999946887 ) ) ;
#16703 = AXIS2_PLACEMENT_3D ( 'NONE', #11717, #4650, #4736 ) ;
#16704 = CARTESIAN_POINT ( 'NONE',  ( 10.56433791484173135, 63.10966569891045452, 8.405314700618397694 ) ) ;
#16705 = CARTESIAN_POINT ( 'NONE',  ( -7.999999999999776179, 0.000000000000000000, -17.32050807568887762 ) ) ;
#16706 = CARTESIAN_POINT ( 'NONE',  ( 12.80285549483701324, 48.58509970421081903, -4.305323710473574650 ) ) ;
#16707 = CARTESIAN_POINT ( 'NONE',  ( 9.520470885617715595, 26.13000000000001322, 6.917026985038135400 ) ) ;
#16708 = ORIENTED_EDGE ( 'NONE', *, *, #6025, .T. ) ;
#16709 = CARTESIAN_POINT ( 'NONE',  ( -11.76794919243112325, 68.77999999999998693, -3.823638476888998827 ) ) ;
#16710 = CARTESIAN_POINT ( 'NONE',  ( -8.043339635997654113, -3.156249999999973355, 8.043339635996304082 ) ) ;
#16711 = CARTESIAN_POINT ( 'NONE',  ( 11.37500000000039435, -84.29062499999980673, -4.711679271993003404 ) ) ;
#16712 = CARTESIAN_POINT ( 'NONE',  ( -13.49999999999999822, 8.079999999999996518, 4.386415899144235908 ) ) ;
#16713 = CARTESIAN_POINT ( 'NONE',  ( -0.1651247708450846174, 43.18593718442633644, -13.49902517774528121 ) ) ;
#16714 = CARTESIAN_POINT ( 'NONE',  ( -7.686450350229677930, 80.93000000000000682, -9.894994522817997407 ) ) ;
#16715 = CARTESIAN_POINT ( 'NONE',  ( 10.92172942406179104, -1.269999999999993356, -7.935100905948385908 ) ) ;
#16716 = CARTESIAN_POINT ( 'NONE',  ( 18.62499999999934985, -32.25937499999992042, 7.714727599200467800 ) ) ;
#16717 = CARTESIAN_POINT ( 'NONE',  ( 5.737830409276838850, 65.88864550709209311, 12.21995698880643033 ) ) ;
#16718 = CARTESIAN_POINT ( 'NONE',  ( 8.343458848123578520, 80.98000000000000398, 11.48378591275254124 ) ) ;
#16719 = CARTESIAN_POINT ( 'NONE',  ( 3.636496289402154414, 51.82999999999999829, 11.19198476289190936 ) ) ;
#16720 = CARTESIAN_POINT ( 'NONE',  ( -3.636496289402155746, 57.53000000000000114, 11.19198476289190936 ) ) ;
#16721 = CARTESIAN_POINT ( 'NONE',  ( -12.76930904997713156, 47.08985268192056139, 4.436624044834727165 ) ) ;
#16722 = CARTESIAN_POINT ( 'NONE',  ( 7.390077773784788029, 45.90380094779195019, -11.29772916998646082 ) ) ;
#16723 = CARTESIAN_POINT ( 'NONE',  ( 8.235194954453712413, 69.86653683069012288, -10.69767531060790411 ) ) ;
#16724 = CARTESIAN_POINT ( 'NONE',  ( -12.00000000000000000, 7.063974596215567558, -2.718289652585034772E-15 ) ) ;
#16725 = CARTESIAN_POINT ( 'NONE',  ( 11.37021635130157193, 30.70260312621314114, -7.278164904536309265 ) ) ;
#16726 = CARTESIAN_POINT ( 'NONE',  ( -12.61460509225905469, 56.10455132028842939, 4.816691950414491608 ) ) ;
#16727 = CARTESIAN_POINT ( 'NONE',  ( 12.50000000000000000, 98.93000000000002103, -8.999999999999996447 ) ) ;
#16728 = CARTESIAN_POINT ( 'NONE',  ( 8.224496495406899754, 32.99287750037110101, 10.71474172343057418 ) ) ;
#16729 = CARTESIAN_POINT ( 'NONE',  ( 2.179318118133371396, 43.10175688752104861, -13.33106788021510170 ) ) ;
#16730 = CARTESIAN_POINT ( 'NONE',  ( 11.92056541865597552, 39.66423766693483799, -6.336564188155583643 ) ) ;
#16731 = ORIENTED_EDGE ( 'NONE', *, *, #3986, .T. ) ;
#16732 = CARTESIAN_POINT ( 'NONE',  ( -13.23734937081763441, 61.83645944859667765, -2.650051958897696291 ) ) ;
#16733 = ORIENTED_EDGE ( 'NONE', *, *, #7636, .T. ) ;
#16734 = CIRCLE ( 'NONE', #6597, 9.500000000000021316 ) ;
#16735 = CARTESIAN_POINT ( 'NONE',  ( -13.01978223802976586, 40.80262089499887423, -3.568884022696015457 ) ) ;
#16736 = CARTESIAN_POINT ( 'NONE',  ( 8.343458848123583849, 30.88000000000000256, -11.48378591275253768 ) ) ;
#16737 = CARTESIAN_POINT ( 'NONE',  ( 18.62500000000000000, -90.49999999999980105, 1.560692158462880521E-12 ) ) ;
#16738 = CARTESIAN_POINT ( 'NONE',  ( 7.242907880593060455, 47.95007431297908340, 11.39473409803327364 ) ) ;
#16739 = CARTESIAN_POINT ( 'NONE',  ( 1.163414459189988049E-15, 0.000000000000000000, -9.500000000000021316 ) ) ;
#16740 = CARTESIAN_POINT ( 'NONE',  ( -8.343458848123576743, 37.48000000000000398, -11.48378591275254301 ) ) ;
#16741 = CARTESIAN_POINT ( 'NONE',  ( -6.730857453137529589, 46.42855663549063649, -11.71077594071010175 ) ) ;
#16742 = CYLINDRICAL_SURFACE ( 'NONE', #10799, 13.50000000000000000 ) ;
#16743 = CARTESIAN_POINT ( 'NONE',  ( 11.37500000000000178, -26.04999999999992255, 9.531744055041752924E-13 ) ) ;
#16744 = CARTESIAN_POINT ( 'NONE',  ( 3.386863761717139543, 53.80170893590585024, 13.06840027907492896 ) ) ;
#16745 = EDGE_CURVE ( 'NONE', #4394, #13814, #6711, .T. ) ;
#16746 = ORIENTED_EDGE ( 'NONE', *, *, #8957, .T. ) ;
#16747 = CARTESIAN_POINT ( 'NONE',  ( -10.32063999273022326, 64.59629040487352825, -8.702553484448552368 ) ) ;
#16748 = ORIENTED_EDGE ( 'NONE', *, *, #10188, .T. ) ;
#16749 = CARTESIAN_POINT ( 'NONE',  ( 5.353457224253611813, 66.98621323793007321, -12.39317060446911967 ) ) ;
#16750 = CARTESIAN_POINT ( 'NONE',  ( -4.936293861523779469, 34.35799467113207584, -12.56715012188039005 ) ) ;
#16751 = CARTESIAN_POINT ( 'NONE',  ( 11.37500000000000000, -16.64999999999995950, 9.531744055041752924E-13 ) ) ;
#16752 = CARTESIAN_POINT ( 'NONE',  ( 9.121473061620024581, 78.03498488587622717, 9.953345307906628747 ) ) ;
#16753 = DIRECTION ( 'NONE',  ( -0.000000000000000000, 1.000000000000000000, -0.000000000000000000 ) ) ;
#16754 = CARTESIAN_POINT ( 'NONE',  ( -5.281055406448098636E-10, 61.18000001472334759, -13.50000000000000000 ) ) ;
#16755 = CARTESIAN_POINT ( 'NONE',  ( 7.500000000000002665, -27.00452558693061533, 5.560661329642322848 ) ) ;
#16756 = CARTESIAN_POINT ( 'NONE',  ( 10.71547152722203577, 72.11813116212451291, 8.211678772859000830 ) ) ;
#16757 = CARTESIAN_POINT ( 'NONE',  ( 7.808600061905294432, 66.88559930404900911, -11.01255116201771322 ) ) ;
#16758 = CARTESIAN_POINT ( 'NONE',  ( -3.636496289402156190, 28.53000000000000114, 11.19198476289190758 ) ) ;
#16759 = CARTESIAN_POINT ( 'NONE',  ( -8.691771469529815392E-16, 59.67999999999999972, 14.19474002721660355 ) ) ;
#16760 = CARTESIAN_POINT ( 'NONE',  ( -8.922957351717846208, 52.52544829913193780, -10.13084569921777245 ) ) ;
#16761 = CARTESIAN_POINT ( 'NONE',  ( -7.272992578804310604, 42.37999999999999545, 10.01041549318726709 ) ) ;
#16762 = CARTESIAN_POINT ( 'NONE',  ( 3.636496289402154414, -16.16999999999999815, 11.19198476289190758 ) ) ;
#16763 = CARTESIAN_POINT ( 'NONE',  ( 8.343458848123583849, 53.87999999999999545, -11.48378591275253768 ) ) ;
#16764 = DIRECTION ( 'NONE',  ( 0.000000000000000000, 0.000000000000000000, 1.000000000000000000 ) ) ;
#16765 = CARTESIAN_POINT ( 'NONE',  ( 11.76794919243112325, -6.720000000000000639, 3.823638476888996163 ) ) ;
#16766 = CARTESIAN_POINT ( 'NONE',  ( -8.716794836091771970, 68.34431102336125718, 10.30886911067118383 ) ) ;
#16767 = CARTESIAN_POINT ( 'NONE',  ( -18.62500000000000000, -8.324999999999979750, -1.562973063126292555E-12 ) ) ;
#16768 = CARTESIAN_POINT ( 'NONE',  ( -10.92172942406179104, 5.230000000000012861, 7.935100905948385908 ) ) ;
#16769 = CARTESIAN_POINT ( 'NONE',  ( 13.16986379960055054, -2.081249999999994937, -13.16986379959834430 ) ) ;
#16770 = CARTESIAN_POINT ( 'NONE',  ( -13.38710100722418517, 73.86912270389885293, -1.743691519651368482 ) ) ;
#16771 = CARTESIAN_POINT ( 'NONE',  ( -3.850178509532386162, 76.31819692911250286, -12.94203568557863093 ) ) ;
#16772 = DIRECTION ( 'NONE',  ( 0.000000000000000000, 0.000000000000000000, -1.000000000000000000 ) ) ;
#16773 = CARTESIAN_POINT ( 'NONE',  ( -12.50000000000000000, 98.93000000000002103, 1.224646799147353059E-15 ) ) ;
#16774 = CARTESIAN_POINT ( 'NONE',  ( -4.171729424061787483, 26.32999999999999119, -12.83926296998457417 ) ) ;
#16775 = CARTESIAN_POINT ( 'NONE',  ( -11.76794919243112325, -2.069999999999995399, -2.602085213965210642E-15 ) ) ;
#16776 = CARTESIAN_POINT ( 'NONE',  ( -3.636496289402153081, 38.32999999999999829, -11.19198476289190936 ) ) ;
#16777 = LINE ( 'NONE', #4686, #5376 ) ;
#16778 = CARTESIAN_POINT ( 'NONE',  ( -4.323434683657179534, 32.52454116264976136, 12.78932864227422961 ) ) ;
#16779 = CARTESIAN_POINT ( 'NONE',  ( 2.928306355011590867, 74.78528128570572164, 13.18019578819992965 ) ) ;
#16780 = B_SPLINE_CURVE_WITH_KNOTS ( 'NONE', 3,
 ( #8518, #4345, #8254, #10807, #9494, #3092, #11070, #16170, #15099, #8164, #2998, #1329, #13528, #12480, #6835, #12211, #13697, #5510 ),
 .UNSPECIFIED., .F., .F.,
 ( 4, 2, 2, 2, 2, 2, 2, 2, 4 ),
 ( 2.344023999656933974E-07, 0.0005273255500080974807, 0.001054416697616229401, 0.001581507845224361213, 0.002108598992832493024, 0.002635690140440624836, 0.003162781288048756214, 0.003689872435656887592, 0.004216963583265018536 ),
 .UNSPECIFIED. ) ;
#16781 = DIRECTION ( 'NONE',  ( 0.000000000000000000, 0.000000000000000000, -1.000000000000000000 ) ) ;
#16782 = B_SPLINE_CURVE_WITH_KNOTS ( 'NONE', 3,
 ( #16238, #9559, #1397, #16423, #8234, #4419, #10783, #9828, #13595, #1490, #5399, #4056, #6905, #9471, #14819, #13763, #2713, #13506, #12281, #176, #5582, #6813, #12190, #10963, #4327, #9735, #7078, #12462 ),
 .UNSPECIFIED., .F., .F.,
 ( 4, 2, 2, 2, 2, 2, 2, 2, 2, 2, 2, 2, 2, 4 ),
 ( 0.000000000000000000, 0.002887961676760914323, 0.004331942515141372352, 0.005775923353521831248, 0.007219904191902289277, 0.008663885030282746438, 0.01155184670704366423, 0.01299582754542412399, 0.01443980838380458376, 0.01588378922218504352, 0.01732777006056550329, 0.02021573173732642628, 0.02165971257570688605, 0.02310369341408734928 ),
 .UNSPECIFIED. ) ;
#16783 = CARTESIAN_POINT ( 'NONE',  ( -7.272992578804310604, 33.38000000000000256, 10.01041549318726709 ) ) ;
#16784 = CARTESIAN_POINT ( 'NONE',  ( 13.36170813389851197, 51.36230533087536543, 1.932902813768764050 ) ) ;
#16785 = CARTESIAN_POINT ( 'NONE',  ( -5.837778096380199955, 38.46761885147301996, 12.18200262067380457 ) ) ;
#16786 = CARTESIAN_POINT ( 'NONE',  ( -17.42428528562871293, 5.918584287042171432, 19.29752010712834220 ) ) ;
#16787 = EDGE_CURVE ( 'NONE', #3760, #4199, #6045, .T. ) ;
#16788 = CYLINDRICAL_SURFACE ( 'NONE', #2879, 26.00000000000000355 ) ;
#16789 = CARTESIAN_POINT ( 'NONE',  ( 0.000000000000000000, 9.999999999999998224, 0.000000000000000000 ) ) ;
#16790 = CARTESIAN_POINT ( 'NONE',  ( 10.66875493928293039, 63.11551852611936653, 8.272111270540923655 ) ) ;
#16791 = CARTESIAN_POINT ( 'NONE',  ( 8.318623314510984912, 41.99726840119479476, 10.63253519692205629 ) ) ;
#16792 = CARTESIAN_POINT ( 'NONE',  ( 12.25765341302126110, 48.63724817142107781, -5.656850844412786294 ) ) ;
#16793 = CARTESIAN_POINT ( 'NONE',  ( -9.520470885617717371, 19.22999999999999687, 6.917026985038133624 ) ) ;
#16794 = ORIENTED_EDGE ( 'NONE', *, *, #2855, .F. ) ;
#16795 = CARTESIAN_POINT ( 'NONE',  ( 11.76794919243112680, 70.57999999999999829, -3.823638476888993942 ) ) ;
#16796 = CARTESIAN_POINT ( 'NONE',  ( -11.37500000000000178, -34.37499999999990052, -9.545674412382054647E-13 ) ) ;
#16797 = CARTESIAN_POINT ( 'NONE',  ( 11.37499999999960210, -32.25937499999992042, 4.711679271994917428 ) ) ;
#16798 = CARTESIAN_POINT ( 'NONE',  ( -0.1166564124115501977, 43.18419448930665538, -13.49957111512055796 ) ) ;
#16799 = CARTESIAN_POINT ( 'NONE',  ( -10.79499759444373019, 80.93000000000004945, -5.634798678252804116 ) ) ;
#16800 = CARTESIAN_POINT ( 'NONE',  ( -13.16986379959834252, -72.84374999999981526, -13.16986379960055054 ) ) ;
#16801 = CARTESIAN_POINT ( 'NONE',  ( 11.80469282007272014, 66.18718478032059238, 6.549751504643047895 ) ) ;
#16802 = FACE_OUTER_BOUND ( 'NONE', #6770, .T. ) ;
#16803 = B_SPLINE_CURVE_WITH_KNOTS ( 'NONE', 3,
 ( #4130, #9542, #2785, #8216, #11033, #13920, #1814, #246, #16492, #6000, #11383, #15154, #1556, #12352, #16669, #16755, #4663, #7061, #3052, #12443, #5912, #7145, #8567, #12531, #2962, #8481, #11208, #12703, #15244, #7228, #13745, #417, #12616, #8392, #5737, #14009, #10070, #15421, #16582, #4487, #8306, #11118, #4576, #4397 ),
 .UNSPECIFIED., .F., .F.,
 ( 4, 2, 2, 2, 2, 2, 2, 2, 2, 2, 2, 2, 2, 2, 2, 2, 2, 2, 2, 2, 2, 4 ),
 ( 0.03689401835950766734, 0.03766257893388839928, 0.03843113950826912428, 0.03919970008264984929, 0.03996826065703058123, 0.04073682123141131317, 0.04150538180579203817, 0.04304250295455348818, 0.04457962410331494513, 0.04611674525207639513, 0.04765386640083785208, 0.04919098754959930209, 0.05072810869836075209, 0.05226522984712220210, 0.05380235099588365211, 0.05533947214464510905, 0.05687659329340655906, 0.05764515386778727712, 0.05841371444216800213, 0.05995083559092944520, 0.06071939616531016326, 0.06148795673969088132 ),
 .UNSPECIFIED. ) ;
#16804 = CARTESIAN_POINT ( 'NONE',  ( 2.272985001014427788E-15, 50.17999999999999261, -12.37355403259654985 ) ) ;
#16805 = CARTESIAN_POINT ( 'NONE',  ( 2.138189944381262642, 8.103118577679731871, -13.49999999999999112 ) ) ;
#16806 = CARTESIAN_POINT ( 'NONE',  ( -12.49416858534635999, 46.74394383384145613, -5.114026567592828698 ) ) ;
#16807 = CARTESIAN_POINT ( 'NONE',  ( 7.279436909953497015, 45.90853851008816378, -11.36958811381530232 ) ) ;
#16808 = CARTESIAN_POINT ( 'NONE',  ( 4.299690572160308814E-08, 62.68000119825558869, 13.49999999999999822 ) ) ;
#16809 = CARTESIAN_POINT ( 'NONE',  ( -18.99999999999998224, 7.773118517290098062, -1.732050807569074147 ) ) ;
#16810 = CARTESIAN_POINT ( 'NONE',  ( 13.41720521117808929, 30.48325862006828402, -1.529750345770487741 ) ) ;
#16811 = CARTESIAN_POINT ( 'NONE',  ( -11.15922986944817197, 56.21581637754891858, 7.597592024288784884 ) ) ;
#16812 = EDGE_CURVE ( 'NONE', #902, #15411, #11642, .T. ) ;
#16813 = DIRECTION ( 'NONE',  ( 0.000000000000000000, 0.000000000000000000, -1.000000000000000000 ) ) ;
#16814 = CARTESIAN_POINT ( 'NONE',  ( 11.16148123762422628, 33.14429372490298675, 7.594972696243417865 ) ) ;
#16815 = CARTESIAN_POINT ( 'NONE',  ( 2.847325915738560642, 43.07762279006870898, -13.19636507075122722 ) ) ;
#16816 = CARTESIAN_POINT ( 'NONE',  ( 8.038493034308670460, 39.87539040871880047, -10.84611687539693570 ) ) ;
#16817 = VERTEX_POINT ( 'NONE', #3416 ) ;
#16818 = CARTESIAN_POINT ( 'NONE',  ( -13.22883851915415931, 62.02637491379582713, 2.727007129524784190 ) ) ;
#16819 = VECTOR ( 'NONE', #5883, 1000.000000000000000 ) ;
#16820 = VERTEX_POINT ( 'NONE', #11556 ) ;
#16821 = ORIENTED_EDGE ( 'NONE', *, *, #3652, .T. ) ;
#16822 = CARTESIAN_POINT ( 'NONE',  ( -8.549982208541774191E-16, 32.68000000000000682, 14.19474002721660355 ) ) ;
#16823 = CARTESIAN_POINT ( 'NONE',  ( 18.62500000000000000, 0.000000000000000000, 1.560692158462880521E-12 ) ) ;
#16824 = CARTESIAN_POINT ( 'NONE',  ( 10.79078081101559405, 48.12244929535420823, 8.112457044903750969 ) ) ;
#16825 = CARTESIAN_POINT ( 'NONE',  ( 9.466621069669054478, 57.80831407961003521, -9.633577061845073786 ) ) ;
#16826 = CARTESIAN_POINT ( 'NONE',  ( 9.237178716131806411, 78.81937718674274151, -9.845633059447870039 ) ) ;
#16827 = CARTESIAN_POINT ( 'NONE',  ( -7.576616670048093940E-16, 78.67999999999999261, 12.37355403259654985 ) ) ;
#16828 = CARTESIAN_POINT ( 'NONE',  ( 8.343458848123583849, 38.87999999999999545, -11.48378591275253768 ) ) ;
#16829 = CARTESIAN_POINT ( 'NONE',  ( 12.70176803441796309, 1.934905186679871999E-15, -0.6935314968477440667 ) ) ;
#16830 = VECTOR ( 'NONE', #7356, 1000.000000000000000 ) ;
#16831 = CARTESIAN_POINT ( 'NONE',  ( -5.935378987246981985, 46.39625066269702813, -12.12563720457925420 ) ) ;
#16832 = CARTESIAN_POINT ( 'NONE',  ( -0.1216187211892394704, 67.18437295985889079, -13.49945684472638341 ) ) ;
#16833 = CARTESIAN_POINT ( 'NONE',  ( 4.711679271993006957, -39.57812499999989342, 11.37500000000039613 ) ) ;
#16834 = EDGE_CURVE ( 'NONE', #4566, #2740, #9707, .T. ) ;
#16835 = CARTESIAN_POINT ( 'NONE',  ( 3.151125265860354574, 53.79336584747739636, 13.12739497994581761 ) ) ;
#16836 = VERTEX_POINT ( 'NONE', #1023 ) ;
#16837 = CYLINDRICAL_SURFACE ( 'NONE', #9528, 13.50000000000000000 ) ;
#16838 = ORIENTED_EDGE ( 'NONE', *, *, #6355, .T. ) ;
#16839 = CARTESIAN_POINT ( 'NONE',  ( 3.704057111973126037, 67.04671062878161081, -12.98374603455249598 ) ) ;
#16840 = CARTESIAN_POINT ( 'NONE',  ( -10.13763839362155217, 34.58653844640922870, -8.915099634223262015 ) ) ;
#16841 = CARTESIAN_POINT ( 'NONE',  ( 4.171729424061791924, 17.03000000000001890, -12.83926296998457239 ) ) ;
#16842 = CARTESIAN_POINT ( 'NONE',  ( -4.711679271994916540, -78.04687499999982947, 11.37499999999960210 ) ) ;
#16843 = CARTESIAN_POINT ( 'NONE',  ( 1.887356908845042813, 77.74786259742627692, 13.36790284719159594 ) ) ;
#16844 = CARTESIAN_POINT ( 'NONE',  ( -8.778540386818084684, 59.34177203136455603, 10.26563256713212446 ) ) ;
#16845 = CARTESIAN_POINT ( 'NONE',  ( 15.34225977864770485, 8.027996330223285071, 9.656730951920737382 ) ) ;
#16846 = CARTESIAN_POINT ( 'NONE',  ( 2.902084407815607718E-14, 5.180000000000006821, -13.50000000000000000 ) ) ;
#16847 = CARTESIAN_POINT ( 'NONE',  ( 11.91185185119470979, 72.66488878920632999, -6.352778759434507094 ) ) ;
#16848 = CARTESIAN_POINT ( 'NONE',  ( 7.960069242295579883, 66.87890050241821882, -10.90399355178459828 ) ) ;
#16849 = CARTESIAN_POINT ( 'NONE',  ( 7.272992578804311492, 26.88000000000001677, -10.01041549318726709 ) ) ;
#16850 = CARTESIAN_POINT ( 'NONE',  ( -10.92172942406178926, 55.62999999999999545, -7.935100905948389460 ) ) ;
#16851 = CARTESIAN_POINT ( 'NONE',  ( -8.971737691618042021, 52.52777621585467926, -10.08760936789154528 ) ) ;
#16852 = CARTESIAN_POINT ( 'NONE',  ( -9.520470885617717371, -16.76999999999999957, 6.917026985038133624 ) ) ;
#16853 = CARTESIAN_POINT ( 'NONE',  ( 4.171729424061789260, 52.83000000000000540, 12.83926296998457417 ) ) ;
#16854 = CARTESIAN_POINT ( 'NONE',  ( 18.46851087777847411, 7.924527533097220022, -1.297848593170553233 ) ) ;
#16855 = CARTESIAN_POINT ( 'NONE',  ( -9.520470885617717371, -1.769999999999993801, 6.917026985038133624 ) ) ;
#16856 = CARTESIAN_POINT ( 'NONE',  ( -9.151681567251712224, 68.32366095331082079, 9.928819553262187014 ) ) ;
#16857 = CARTESIAN_POINT ( 'NONE',  ( 18.62499999999934630, -48.90937499999989058, 7.714727599200467800 ) ) ;
#16858 = CARTESIAN_POINT ( 'NONE',  ( 13.49999999999999822, 71.28000000000000114, 4.386415899144236796 ) ) ;
#16859 = CARTESIAN_POINT ( 'NONE',  ( 7.714727599197338748, -46.82812499999989342, 18.62500000000063949 ) ) ;
#16860 = CARTESIAN_POINT ( 'NONE',  ( -5.113724666901518390, 65.49524033223701736, 12.49402144522741054 ) ) ;
#16861 = CARTESIAN_POINT ( 'NONE',  ( -11.72372701389734040, 80.92999999999994998, -2.238432065937304039 ) ) ;
#16862 = CARTESIAN_POINT ( 'NONE',  ( -4.171729424061787483, 2.329999999999998739, -12.83926296998457417 ) ) ;
#16863 = EDGE_LOOP ( 'NONE', ( #15024, #17097, #14502, #11705, #9756, #9875, #7140, #6750, #3998, #5993, #13198, #11244, #1878, #5049, #2301, #11359, #1273, #243, #456, #1330, #10830, #7995, #9804, #5773, #14349, #13401, #4468, #14077, #13914, #12510, #3734, #7844, #5378, #836, #4812, #2671, #4700 ) ) ;
#16864 = CARTESIAN_POINT ( 'NONE',  ( -9.520470885617715595, 35.62999999999999545, -6.917026985038136289 ) ) ;
#16865 = CARTESIAN_POINT ( 'NONE',  ( 10.92172942406179104, 80.72999999999998977, -7.935100905948385908 ) ) ;
#16866 = CARTESIAN_POINT ( 'NONE',  ( -13.27449558559234966, 31.84307581624048211, -2.469241552857083466 ) ) ;
#16867 = CARTESIAN_POINT ( 'NONE',  ( 7.249350209789888311, 74.95018326669271858, 11.39098842421434910 ) ) ;
#16868 = LINE ( 'NONE', #614, #6865 ) ;
#16869 = ADVANCED_FACE ( 'NONE', ( #6434 ), #2072, .F. ) ;
#16870 =( NAMED_UNIT ( * ) SI_UNIT ( $, .STERADIAN. ) SOLID_ANGLE_UNIT ( ) );
#16871 = CARTESIAN_POINT ( 'NONE',  ( 5.883994266285501595, 30.92926174983937671, 10.19133159454443494 ) ) ;
#16872 = CARTESIAN_POINT ( 'NONE',  ( 12.53676505969797716, 51.61201439350722353, -5.009677754619692891 ) ) ;
#16873 = CARTESIAN_POINT ( 'NONE',  ( -9.374316402762136846, 38.31261403934563248, 9.714543350701456248 ) ) ;
#16874 = CARTESIAN_POINT ( 'NONE',  ( 10.38072545181284490, 36.76044073136390722, -8.630800951527588083 ) ) ;
#16875 = CARTESIAN_POINT ( 'NONE',  ( 11.37499999999960210, -82.20937499999980957, 4.711679271994918317 ) ) ;
#16876 = LINE ( 'NONE', #8775, #10527 ) ;
#16877 = FACE_BOUND ( 'NONE', #4470, .T. ) ;
#16878 = CARTESIAN_POINT ( 'NONE',  ( -4.025269380572474631, 80.53526585944453586, 12.88604957218887392 ) ) ;
#16879 = CARTESIAN_POINT ( 'NONE',  ( 3.088727648909929346, 41.79106320569731992, 13.14190891410004447 ) ) ;
#16880 = CARTESIAN_POINT ( 'NONE',  ( 13.49572376180440614, 48.41833269112186144, 0.3397958042547450930 ) ) ;
#16881 = CARTESIAN_POINT ( 'NONE',  ( -11.76794919243112325, 12.92999999999999616, -2.602085213965210642E-15 ) ) ;
#16882 = ORIENTED_EDGE ( 'NONE', *, *, #14546, .T. ) ;
#16883 = CARTESIAN_POINT ( 'NONE',  ( 9.520470885617715595, 67.12999999999999545, 6.917026985038134512 ) ) ;
#16884 = CARTESIAN_POINT ( 'NONE',  ( -11.37499999999960743, -16.68437499999993889, -4.711679271994912099 ) ) ;
#16885 = CARTESIAN_POINT ( 'NONE',  ( 0.000000000000000000, 0.000000000000000000, 0.000000000000000000 ) ) ;
#16886 = CARTESIAN_POINT ( 'NONE',  ( -3.636496289402152637, 30.32999999999999474, -11.19198476289190936 ) ) ;
#16887 = CARTESIAN_POINT ( 'NONE',  ( 2.377126426719958996, 76.09455468723297145, -13.29565205172750098 ) ) ;
#16888 = CARTESIAN_POINT ( 'NONE',  ( 3.636496289402154414, 33.82999999999999829, 11.19198476289190936 ) ) ;
#16889 = VECTOR ( 'NONE', #8391, 1000.000000000000000 ) ;
#16890 = CARTESIAN_POINT ( 'NONE',  ( 7.714727599200458030, -69.72187499999984084, -18.62499999999935341 ) ) ;
#16891 = CARTESIAN_POINT ( 'NONE',  ( 5.477308328785983171, 65.87853220268742405, 12.33977219472520126 ) ) ;
#16892 = CARTESIAN_POINT ( 'NONE',  ( 13.50000000000000000, 78.43000000000000682, 1.653273178848926867E-15 ) ) ;
#16893 = ADVANCED_FACE ( 'NONE', ( #5105 ), #10497, .F. ) ;
#16894 = CARTESIAN_POINT ( 'NONE',  ( 9.520470885617717371, 52.72999999999999687, -6.917026985038131848 ) ) ;
#16895 = CARTESIAN_POINT ( 'NONE',  ( -13.20223561047976268, 59.02975874724325678, 2.819883426483977829 ) ) ;
#16896 = CARTESIAN_POINT ( 'NONE',  ( 13.16065579104130734, 45.32293695995979732, 3.019718079858381365 ) ) ;
#16897 = CARTESIAN_POINT ( 'NONE',  ( 5.631590942443961190, 69.97548339101035708, -12.26927851611127984 ) ) ;
#16898 =( NAMED_UNIT ( * ) SI_UNIT ( $, .STERADIAN. ) SOLID_ANGLE_UNIT ( ) );
#16899 = CARTESIAN_POINT ( 'NONE',  ( 12.85462009865432620, 30.57980069535864232, -4.171484233273251796 ) ) ;
#16900 = AXIS2_PLACEMENT_3D ( 'NONE', #339, #1745, #514 ) ;
#16901 = CARTESIAN_POINT ( 'NONE',  ( -13.47914357258245133, 55.90410188285380855, -0.7501567218792010161 ) ) ;
#16902 = CARTESIAN_POINT ( 'NONE',  ( -8.891200544363830713E-16, 52.67999999999999972, 13.50000000000000000 ) ) ;
#16903 = CARTESIAN_POINT ( 'NONE',  ( 2.696128579769775158, 64.08305753458944309, -13.22804826153012314 ) ) ;
#16904 = CARTESIAN_POINT ( 'NONE',  ( 22.26879735319529274, 6.548268786306342015, -7.999999999999943157 ) ) ;
#16905 = CARTESIAN_POINT ( 'NONE',  ( 13.01577231705888593, 39.55791707290476467, -3.583317184063302907 ) ) ;
#16906 = ORIENTED_EDGE ( 'NONE', *, *, #4067, .T. ) ;
#16907 = CARTESIAN_POINT ( 'NONE',  ( -12.92483791310288055, 62.06981881790770217, 3.901126829718378097 ) ) ;
#16908 = ORIENTED_EDGE ( 'NONE', *, *, #12907, .F. ) ;
#16909 = ORIENTED_EDGE ( 'NONE', *, *, #5806, .F. ) ;
#16910 = CARTESIAN_POINT ( 'NONE',  ( -8.343458848123582072, 29.38000000000000611, 11.48378591275254124 ) ) ;
#16911 = CARTESIAN_POINT ( 'NONE',  ( -13.16986379959834252, -6.243749999999985256, -13.16986379960055054 ) ) ;
#16912 = CARTESIAN_POINT ( 'NONE',  ( 2.397835237309143608, 58.09378275998017926, -13.28536204613238425 ) ) ;
#16913 = CARTESIAN_POINT ( 'NONE',  ( 10.92279921418927202, 78.72993820095271644, -7.933666610018733856 ) ) ;
#16914 = CARTESIAN_POINT ( 'NONE',  ( -9.520470885617715595, 80.63000000000000966, -6.917026985038136289 ) ) ;
#16915 = CARTESIAN_POINT ( 'NONE',  ( 8.343458848123583849, 41.88000000000000256, -11.48378591275253768 ) ) ;
#16916 = CARTESIAN_POINT ( 'NONE',  ( -3.636496289402153081, 83.32999999999999829, -11.19198476289190936 ) ) ;
#16917 = EDGE_CURVE ( 'NONE', #5051, #4482, #15948, .T. ) ;
#16918 = LINE ( 'NONE', #4909, #5069 ) ;
#16919 = CARTESIAN_POINT ( 'NONE',  ( -12.50000000000000000, -18.00000000000000355, 8.999999999999998224 ) ) ;
#16920 = CARTESIAN_POINT ( 'NONE',  ( -2.138189944381240881, 34.60311857767972299, 13.49999999999999822 ) ) ;
#16921 = CARTESIAN_POINT ( 'NONE',  ( -8.043339635997654113, -3.156249999999973355, 8.043339635996304082 ) ) ;
#16922 = CARTESIAN_POINT ( 'NONE',  ( 1.281066422249921066, 53.72599284319046120, 13.44791089454055211 ) ) ;
#16923 = EDGE_LOOP ( 'NONE', ( #16193, #14632, #373, #6150, #3494, #14521, #3579, #9610 ) ) ;
#16924 = CARTESIAN_POINT ( 'NONE',  ( -1.732050807568877859, 7.773118517290099838, -18.99999999999999645 ) ) ;
#16925 = ORIENTED_EDGE ( 'NONE', *, *, #5661, .F. ) ;
#16926 = CARTESIAN_POINT ( 'NONE',  ( 0.000000000000000000, 3.000000000000000000, -22.50000000000000355 ) ) ;
#16927 = CARTESIAN_POINT ( 'NONE',  ( -11.37499999999999645, -15.57499999999997975, -9.545674412382054647E-13 ) ) ;
#16928 = CARTESIAN_POINT ( 'NONE',  ( 10.00000000000002132, 0.000000000000000000, -17.32050807568876394 ) ) ;
#16929 = CARTESIAN_POINT ( 'NONE',  ( -2.585177345473597121, 59.58711577648321622, 13.25618079341042410 ) ) ;
#16930 = CARTESIAN_POINT ( 'NONE',  ( 0.000000000000000000, 108.9300000000000068, 0.000000000000000000 ) ) ;
#16931 = DIRECTION ( 'NONE',  ( 0.000000000000000000, 0.000000000000000000, 1.000000000000000000 ) ) ;
#16932 = AXIS2_PLACEMENT_3D ( 'NONE', #16668, #14008, #7496 ) ;
#16933 = CARTESIAN_POINT ( 'NONE',  ( 11.89247718313613333, 72.66634291386961308, -6.389002466017593918 ) ) ;
#16934 = CARTESIAN_POINT ( 'NONE',  ( 2.279995255611139653E-15, 30.18000000000001393, -12.37355403259654985 ) ) ;
#16935 = CARTESIAN_POINT ( 'NONE',  ( -4.171729424061791036, 56.52999999999999403, 12.83926296998457239 ) ) ;
#16936 = CARTESIAN_POINT ( 'NONE',  ( -5.804184846681112120, 52.39123887527535572, -12.18857870861379489 ) ) ;
#16937 = EDGE_CURVE ( 'NONE', #9259, #11282, #7342, .T. ) ;
#16938 = CARTESIAN_POINT ( 'NONE',  ( 13.50000000000000000, 77.42999999999999261, 1.653273178848926867E-15 ) ) ;
#16939 = CARTESIAN_POINT ( 'NONE',  ( 13.16986379959834075, -97.81874999999976694, 13.16986379960055231 ) ) ;
#16940 = CARTESIAN_POINT ( 'NONE',  ( -4.700540564771944929, 68.51070403678419041, 12.65611679705310699 ) ) ;
#16941 = CARTESIAN_POINT ( 'NONE',  ( 13.16986379959834075, -47.86874999999988489, 13.16986379960055231 ) ) ;
#16942 = CARTESIAN_POINT ( 'NONE',  ( 1.732050807568739970, 7.773118517290100726, 19.00000000000000355 ) ) ;
#16943 = CARTESIAN_POINT ( 'NONE',  ( 18.62500000000064304, -17.69062499999995453, -7.714727599197335195 ) ) ;
#16944 = CARTESIAN_POINT ( 'NONE',  ( -7.676400182581260445, 65.39140243087504700, 11.10517247809514352 ) ) ;
#16945 = CARTESIAN_POINT ( 'NONE',  ( 7.416407864998737054, 7.846025403784439689, 10.20780970022447853 ) ) ;
#16946 = AXIS2_PLACEMENT_3D ( 'NONE', #6027, #11410, #14295 ) ;
#16947 = CARTESIAN_POINT ( 'NONE',  ( -8.343458848123578520, 2.479999999999999982, -11.48378591275254124 ) ) ;
#16948 = CARTESIAN_POINT ( 'NONE',  ( -13.49999999999999822, 24.08000000000001606, 4.386415899144235908 ) ) ;
#16949 = VERTEX_POINT ( 'NONE', #1278 ) ;
#16950 = CARTESIAN_POINT ( 'NONE',  ( -7.272992578804307939, 32.47999999999999687, -10.01041549318727064 ) ) ;
#16951 = CARTESIAN_POINT ( 'NONE',  ( -11.00000000000012612, 7.773118517290097174, 15.58845726811980725 ) ) ;
#16952 = CARTESIAN_POINT ( 'NONE',  ( -2.023567624813612298, 40.25271813351103845, -13.35527371537015107 ) ) ;
#16953 = CARTESIAN_POINT ( 'NONE',  ( -12.15799536072682230, 31.71389791688402582, -5.884964112094992927 ) ) ;
#16954 = CARTESIAN_POINT ( 'NONE',  ( 6.028239964215877045, 74.90006706535075409, 12.07938228801198122 ) ) ;
#16955 = CARTESIAN_POINT ( 'NONE',  ( 10.13447305563719603, 60.08610105333452367, 8.928467604290379001 ) ) ;
#16956 = CARTESIAN_POINT ( 'NONE',  ( 2.138189944381242213, 4.103118577679734535, -13.49999999999999822 ) ) ;
#16957 = CARTESIAN_POINT ( 'NONE',  ( 8.343458848123578520, 76.98000000000000398, 11.48378591275254124 ) ) ;
#16958 = CARTESIAN_POINT ( 'NONE',  ( 13.50024950918025901, 51.42556551580268831, 0.1251884723271639854 ) ) ;
#16959 =( BOUNDED_CURVE ( )  B_SPLINE_CURVE ( 2, ( #5421, #1332, #16173, #2915, #12214, #9326, #2564, #16356, #6748, #199, #1512, #10809, #6927, #4082, #7994, #12305, #13701, #1251, #5604, #8345, #12395, #4703, #16536, #3277, #12572, #1941, #2028, #7184, #7364, #8694, #9850, #16797, #7453, #8523, #15371, #14054, #9936, #8784, #12654, #12833, #6042, #4350, #459, #11333, #14140, #5868, #5694, #631, #1685, #15197, #544, #12743, #9759, #16447, #15104, #7271, #11425, #3003, #11161, #8433, #3370, #13960, #4443, #7101, #13873, #371, #10108, #12485, #15459, #5953, #1775, #13787, #5776, #11074, #3097, #11247, #8608, #16626, #4529, #15285, #3186, #16711, #1857, #4616, #10023, #3624, #5144, #7710, #973, #6210, #4963, #11769, #800, #15629, #6473, #16973, #3457 ),
 .UNSPECIFIED., .F., .F. ) 
 B_SPLINE_CURVE_WITH_KNOTS ( ( 3, 2, 2, 2, 2, 2, 2, 2, 2, 2, 2, 2, 2, 2, 2, 2, 2, 2, 2, 2, 2, 2, 2, 2, 2, 2, 2, 2, 2, 2, 2, 2, 2, 2, 2, 2, 2, 2, 2, 2, 2, 2, 2, 2, 2, 2, 2, 2, 3 ),
 ( 0.000000000000000000, 0.02083333333333333218, 0.04166666666666666435, 0.06250000000000000000, 0.08333333333333332871, 0.1041666666666666713, 0.1250000000000000000, 0.1458333333333333426, 0.1666666666666666574, 0.1875000000000000000, 0.2083333333333333426, 0.2291666666666666574, 0.2500000000000000000, 0.2708333333333333148, 0.2916666666666666852, 0.3125000000000000000, 0.3333333333333333148, 0.3541666666666666852, 0.3750000000000000000, 0.3958333333333333148, 0.4166666666666666852, 0.4375000000000000000, 0.4583333333333333148, 0.4791666666666666852, 0.5000000000000000000, 0.5208333333333333703, 0.5416666666666666297, 0.5625000000000000000, 0.5833333333333333703, 0.6041666666666666297, 0.6250000000000000000, 0.6458333333333333703, 0.6666666666666666297, 0.6875000000000000000, 0.7083333333333333703, 0.7291666666666666297, 0.7500000000000000000, 0.7708333333333333703, 0.7916666666666666297, 0.8125000000000000000, 0.8333333333333333703, 0.8541666666666666297, 0.8750000000000000000, 0.8958333333333333703, 0.9166666666666666297, 0.9375000000000000000, 0.9583333333333333703, 0.9791666666666666297, 1.000000000000000000 ),
 .UNSPECIFIED. ) 
 CURVE ( )  GEOMETRIC_REPRESENTATION_ITEM ( )  RATIONAL_B_SPLINE_CURVE ( ( 1.000000000000000000, 0.9238795325112867385, 1.000000000000000000, 0.9238795325112867385, 1.000000000000000000, 0.9238795325112867385, 1.000000000000000000, 0.9238795325112867385, 1.000000000000000000, 0.9238795325112867385, 1.000000000000000000, 0.9238795325112867385, 1.000000000000000000, 0.9238795325112867385, 1.000000000000000000, 0.9238795325112867385, 1.000000000000000000, 0.9238795325112867385, 1.000000000000000000, 0.9238795325112867385, 1.000000000000000000, 0.9238795325112867385, 1.000000000000000000, 0.9238795325112867385, 1.000000000000000000, 0.9238795325112867385, 1.000000000000000000, 0.9238795325112867385, 1.000000000000000000, 0.9238795325112867385, 1.000000000000000000, 0.9238795325112867385, 1.000000000000000000, 0.9238795325112867385, 1.000000000000000000, 0.9238795325112867385, 1.000000000000000000, 0.9238795325112867385, 1.000000000000000000, 0.9238795325112867385, 1.000000000000000000, 0.9238795325112867385, 1.000000000000000000, 0.9238795325112867385, 1.000000000000000000, 0.9238795325112867385, 1.000000000000000000, 0.9238795325112867385, 1.000000000000000000, 0.9238795325112867385, 1.000000000000000000, 0.9238795325112867385, 1.000000000000000000, 0.9238795325112867385, 1.000000000000000000, 0.9238795325112867385, 1.000000000000000000, 0.9238795325112867385, 1.000000000000000000, 0.9238795325112867385, 1.000000000000000000, 0.9238795325112867385, 1.000000000000000000, 0.9238795325112867385, 1.000000000000000000, 0.9238795325112867385, 1.000000000000000000, 0.9238795325112867385, 1.000000000000000000, 0.9238795325112867385, 1.000000000000000000, 0.9238795325112867385, 1.000000000000000000, 0.9238795325112867385, 1.000000000000000000, 0.9238795325112867385, 1.000000000000000000, 0.9238795325112867385, 1.000000000000000000, 0.9238795325112867385, 1.000000000000000000, 0.9238795325112867385, 1.000000000000000000, 0.9238795325112867385, 1.000000000000000000, 0.9238795325112867385, 1.000000000000000000, 0.9238795325112867385, 1.000000000000000000, 0.9238795325112867385, 1.000000000000000000, 0.9238795325112867385, 1.000000000000000000, 0.9238795325112867385, 1.000000000000000000, 0.9238795325112867385, 1.000000000000000000 ) ) 
 REPRESENTATION_ITEM ( '' )  );
#16960 = CARTESIAN_POINT ( 'NONE',  ( -13.33762187123810783, 38.00319105045628021, 2.087548345912210834 ) ) ;
#16961 = CARTESIAN_POINT ( 'NONE',  ( 11.96904469129489712, 36.66054586001213522, -6.244362512893062878 ) ) ;
#16962 = CARTESIAN_POINT ( 'NONE',  ( 4.711679271993006957, -20.77812499999997087, 11.37500000000039257 ) ) ;
#16963 = CARTESIAN_POINT ( 'NONE',  ( -8.343458848123578520, 69.47999999999998977, -11.48378591275254124 ) ) ;
#16964 = CARTESIAN_POINT ( 'NONE',  ( -5.742344703206066825, 77.47123319695006671, 12.22553970615274821 ) ) ;
#16965 = CARTESIAN_POINT ( 'NONE',  ( -0.4450458824277843117, 80.66412212204676280, 13.50000000009667822 ) ) ;
#16966 = FACE_OUTER_BOUND ( 'NONE', #3712, .T. ) ;
#16967 = CARTESIAN_POINT ( 'NONE',  ( 13.49520900591351591, 48.41764727028196802, 0.3596711816471687140 ) ) ;
#16968 = CARTESIAN_POINT ( 'NONE',  ( 11.76794919243112325, 11.27999999999999936, 3.823638476888996163 ) ) ;
#16969 = EDGE_CURVE ( 'NONE', #3997, #4960, #4250, .T. ) ;
#16970 = ORIENTED_EDGE ( 'NONE', *, *, #15601, .T. ) ;
#16971 = CARTESIAN_POINT ( 'NONE',  ( -11.76794919243112325, 60.07999999999999119, 3.823638476888994830 ) ) ;
#16972 = CARTESIAN_POINT ( 'NONE',  ( -4.711679271993003404, -31.25312499999991545, -11.37500000000039613 ) ) ;
#16973 = CARTESIAN_POINT ( 'NONE',  ( 11.37499999999960210, -98.85937499999975842, 4.711679271994917428 ) ) ;
#16974 = CARTESIAN_POINT ( 'NONE',  ( 13.50000000000000355, 0.5800000000000020695, -4.386415899144233244 ) ) ;
#16975 = CARTESIAN_POINT ( 'NONE',  ( 9.520470885617715595, 29.13000000000001677, 6.917026985038135400 ) ) ;
#16976 = CARTESIAN_POINT ( 'NONE',  ( -6.155833696456248560, 80.92999999999999261, -11.06015457064562568 ) ) ;
#16977 = CARTESIAN_POINT ( 'NONE',  ( 13.16986379959834075, -31.21874999999992539, 13.16986379960055231 ) ) ;
#16978 = CARTESIAN_POINT ( 'NONE',  ( -12.50000000000000000, -14.00000000000000178, -2.204364238465235822E-15 ) ) ;
#16979 = CARTESIAN_POINT ( 'NONE',  ( 7.272992578804311492, 49.88000000000000256, -10.01041549318726709 ) ) ;
#16980 = FACE_OUTER_BOUND ( 'NONE', #8299, .T. ) ;
#16981 = CARTESIAN_POINT ( 'NONE',  ( -9.664723050658645676, 59.29818881219673443, 9.428350389498694639 ) ) ;
#16982 = CARTESIAN_POINT ( 'NONE',  ( 11.44301261067812980, 45.16219600046670735, 7.162975258549002078 ) ) ;
#16983 = FACE_OUTER_BOUND ( 'NONE', #9263, .T. ) ;
#16984 = CARTESIAN_POINT ( 'NONE',  ( 6.123233995736765296E-16, -1.200000000000000030E-05, -5.000000000000000000 ) ) ;
#16985 = CARTESIAN_POINT ( 'NONE',  ( 13.37541923767974339, 30.36531257111265347, 1.848779302742114883 ) ) ;
#16986 = CARTESIAN_POINT ( 'NONE',  ( -11.56502629853437014, 56.19075719356373355, 6.997501230777822379 ) ) ;
#16987 = CARTESIAN_POINT ( 'NONE',  ( -8.596527567661915725, 50.34992577827640048, 10.40911947817394001 ) ) ;
#16988 = CARTESIAN_POINT ( 'NONE',  ( 5.419104353479628600, 63.98373895619566554, -12.36469703756342575 ) ) ;
#16989 = CARTESIAN_POINT ( 'NONE',  ( 0.7984662603207598464, 43.15138461308531248, -13.47713055834477203 ) ) ;
#16990 = CARTESIAN_POINT ( 'NONE',  ( 11.89842161280430766, 39.66590154200320484, -6.378003534159421228 ) ) ;
#16991 = ORIENTED_EDGE ( 'NONE', *, *, #10327, .F. ) ;
#16992 = CARTESIAN_POINT ( 'NONE',  ( -12.08543674838329096, 61.70855775374815977, -6.016151293341113870 ) ) ;
#16993 = ORIENTED_EDGE ( 'NONE', *, *, #13690, .F. ) ;
#16994 = ORIENTED_EDGE ( 'NONE', *, *, #6120, .F. ) ;
#16995 = CARTESIAN_POINT ( 'NONE',  ( -13.50000000000000000, 31.93000000000001393, -3.469446951953614189E-15 ) ) ;
#16996 = CARTESIAN_POINT ( 'NONE',  ( -1.564113515457998572E-12, -12.48749999999997051, 18.62500000000000000 ) ) ;
#16997 = AXIS2_PLACEMENT_3D ( 'NONE', #5693, #3002, #7100 ) ;
#16998 = CARTESIAN_POINT ( 'NONE',  ( 11.52369798092066766, 57.69241147752207155, -7.032473906922456663 ) ) ;
#16999 = CARTESIAN_POINT ( 'NONE',  ( 5.029662762750280791, 78.99851775006395371, -12.52810838249923542 ) ) ;
#17000 = CARTESIAN_POINT ( 'NONE',  ( -3.636496289402153081, 83.32999999999999829, -11.19198476289190936 ) ) ;
#17001 = CARTESIAN_POINT ( 'NONE',  ( 8.343458848123583849, 1.879999999999997451, -11.48378591275253768 ) ) ;
#17002 = PRODUCT_RELATED_PRODUCT_CATEGORY ( 'part', '', ( #16206 ) ) ;
#17003 = CARTESIAN_POINT ( 'NONE',  ( 11.37637957285810586, -100.0000000000000000, 0.000000000000000000 ) ) ;
#17004 = CARTESIAN_POINT ( 'NONE',  ( -2.838270712586780596E-14, 67.18000000000000682, -13.50000000000000178 ) ) ;
#17005 = CARTESIAN_POINT ( 'NONE',  ( -4.711679271994916540, -54.14687499999985931, 11.37499999999960565 ) ) ;
#17006 = CIRCLE ( 'NONE', #3173, 5.000000000000000000 ) ;
#17007 = CARTESIAN_POINT ( 'NONE',  ( -8.343458848123582072, 73.37999999999999545, 11.48378591275253768 ) ) ;
#17008 = CARTESIAN_POINT ( 'NONE',  ( 9.032813657610146763, 33.82959620145423685, -10.04677253184694763 ) ) ;
#17009 = B_SPLINE_CURVE_WITH_KNOTS ( 'NONE', 3,
 ( #1099, #15758, #11979, #14518, #3758, #10227, #8989, #924, #15583, #5096, #7574, #9170, #7664, #17185, #3668, #7751, #835, #8906, #9081, #1188, #4915, #15935, #14346, #13297, #17270, #7839, #6514, #13041, #6246, #6331, #13212, #6599, #10313, #14610, #14433, #11720, #3491, #2323, #11632, #11895, #15850, #17095, #5184, #14261, #12952, #9257, #5003, #10574, #10401, #17008, #13124, #1013, #2493, #7924, #6424, #4825, #2150, #2669, #9605, #2846, #4102, #13638, #1532, #9518, #16190, #16021, #12147, #5533, #8365, #36, #7038, #12326, #13380, #9430, #6858, #14957, #3928, #10658, #9345, #1440, #219, #6947, #10742, #16106, #1270, #8189, #5355, #6682, #8101, #12064, #5625, #17441, #8277, #12236, #2581, #2757, #17360, #10918, #9692, #5274, #14779, #8013, #11006, #13551, #4016, #128, #6768, #1352, #13466, #14863, #13723, #14694, #16287, #5441, #10828, #4194, #4282, #16377, #15040, #2936, #1621, #2045, #12760, #15303, #11353, #9869, #14072, #478, #11441, #8454, #5799, #12675, #4464, #15219, #16814, #3116, #11182, #4722, #7203, #8543, #8712, #5713, #10123, #15476, #3387, #7290, #9780, #9955, #7120, #16728, #565, #5887, #4635, #11095, #13809, #13893, #3208, #6058, #16558, #1792, #16467, #10042, #8800, #15127, #4372, #3024, #12589, #14157, #648, #13979, #12416, #11267, #304, #1708, #16644, #15391, #4550, #3299, #12507, #8628 ),
 .UNSPECIFIED., .F., .F.,
 ( 4, 2, 2, 2, 2, 2, 2, 2, 2, 2, 2, 2, 1, 2, 2, 2, 2, 1, 1, 1, 2, 2, 2, 1, 1, 2, 2, 2, 2, 2, 2, 1, 2, 2, 2, 2, 2, 1, 2, 2, 2, 1, 2, 2, 1, 1, 1, 2, 2, 2, 2, 1, 2, 2, 2, 2, 2, 2, 1, 2, 2, 1, 1, 1, 2, 2, 2, 2, 2, 2, 1, 1, 1, 2, 1, 2, 2, 2, 2, 1, 2, 2, 1, 2, 2, 1, 2, 2, 2, 2, 2, 2, 1, 2, 2, 2, 2, 2, 2, 2, 1, 1, 1, 4 ),
 ( 0.9166751061640373566, 0.9175942170658361041, 0.9185133279676349627, 0.9187431056930845941, 0.9188005501244470574, 0.9188579945558095208, 0.9189728834185343365, 0.9194324388694337102, 0.9196622165948834526, 0.9197771054576082683, 0.9198058276732895555, 0.9198345498889707317, 0.9198919943203330840, 0.9203515497712325688, 0.9208111052221319426, 0.9208398274378131187, 0.9208541885456537068, 0.9208685496534944059, 0.9209259940848567583, 0.9210408829475815740, 0.9212706606730313164, 0.9221897715748300639, 0.9226493270257294377, 0.9227642158884542534, 0.9228216603198167167, 0.9228503825354978929, 0.9228791047511791801, 0.9231088824766288115, 0.9240279933784276700, 0.9244875488293271548, 0.9247173265547767862, 0.9248322154175017129, 0.9248896598488640652, 0.9249471042802265286, 0.9258662151820253872, 0.9258949373977065633, 0.9259236596133877395, 0.9259811040447502029, 0.9260959929074750185, 0.9263257706329247609, 0.9267853260838241347, 0.9269002149465490614, 0.9269289371622302376, 0.9269361177161505871, 0.9269432982700708257, 0.9269576593779115248, 0.9270151038092739881, 0.9272448815347239526, 0.9277044369856238815, 0.9286235478874236282, 0.9288533256128735927, 0.9289107700442360560, 0.9289394922599173432, 0.9289682144755985194, 0.9290831033383235571, 0.9295426587892234860, 0.9304617696910232327, 0.9309213251419231616, 0.9309787695732856250, 0.9309859501272059745, 0.9309931306811262131, 0.9310074917889669122, 0.9310362140046480883, 0.9311511028673731261, 0.9313808805928230905, 0.9322999914946228373, 0.9327595469455227661, 0.9329893246709727306, 0.9330180468866540178, 0.9330324079944946059, 0.9330467691023351939, 0.9331042135336976573, 0.9332191023964226950, 0.9341382132982226638, 0.9345977687491225927, 0.9348275464745725571, 0.9350573242000225216, 0.9368955460036223482, 0.9371253237290724236, 0.9373551014545223881, 0.9378146569054223169, 0.9387337678072222857, 0.9389635455326722502, 0.9390784343953971769, 0.9391358788267597513, 0.9391933232581222146, 0.9396528787090221435, 0.9405719896108221123, 0.9410315450617221522, 0.9414911005126220811, 0.9424102114144220499, 0.9428697668653219788, 0.9430995445907719432, 0.9431569890221344066, 0.9432144334534969810, 0.9433293223162219077, 0.9442484332180218765, 0.9451675441198218452, 0.9451962663355031324, 0.9452249885511843086, 0.9452824329825468830, 0.9453973218452718097, 0.9456270995707217741, 0.9460866550216218140 ),
 .UNSPECIFIED. ) ;
#17010 = EDGE_CURVE ( 'NONE', #7996, #4811, #16285, .T. ) ;
#17011 = EDGE_LOOP ( 'NONE', ( #3621, #4445, #282, #13172 ) ) ;
#17012 = CARTESIAN_POINT ( 'NONE',  ( 1.653273178848926472E-15, 80.93000000000000682, 13.50000000000000000 ) ) ;
#17013 = EDGE_CURVE ( 'NONE', #16449, #15368, #7369, .T. ) ;
#17014 = ORIENTED_EDGE ( 'NONE', *, *, #6481, .F. ) ;
#17015 = CARTESIAN_POINT ( 'NONE',  ( 16.97418022790852277, 7.854708479871425730, -8.022689779262671905 ) ) ;
#17016 = CARTESIAN_POINT ( 'NONE',  ( 11.37499999999960210, -39.50937499999993463, 4.711679271994916540 ) ) ;
#17017 = CARTESIAN_POINT ( 'NONE',  ( 10.08666879418669993, 78.08365181486860251, 8.984249537996154444 ) ) ;
#17018 = CARTESIAN_POINT ( 'NONE',  ( -6.649684940163065328, 59.43487996509021798, 11.75074814822897018 ) ) ;
#17019 = CARTESIAN_POINT ( 'NONE',  ( 16.47957145870430296, 7.956016782093528583, 8.177092975168907429 ) ) ;
#17020 = CARTESIAN_POINT ( 'NONE',  ( -10.92172942406179104, 6.230000000000012861, 7.935100905948385908 ) ) ;
#17021 = DIRECTION ( 'NONE',  ( 0.000000000000000000, -0.000000000000000000, 1.000000000000000000 ) ) ;
#17022 = CARTESIAN_POINT ( 'NONE',  ( 13.50000000000000000, 54.42999999999999972, 1.653273178848926867E-15 ) ) ;
#17023 = CARTESIAN_POINT ( 'NONE',  ( -3.139671853673947410, 71.56710900613775550, 13.12983489637678680 ) ) ;
#17024 = CARTESIAN_POINT ( 'NONE',  ( 1.732050807568740858, 0.000000000000000000, 19.00000000000000355 ) ) ;
#17025 = CARTESIAN_POINT ( 'NONE',  ( 18.62500000000064659, 6.209375000000004974, -7.714727599197336083 ) ) ;
#17026 = CARTESIAN_POINT ( 'NONE',  ( -5.452081557087118391, 68.48233558703648782, 12.35724791920625165 ) ) ;
#17027 = CARTESIAN_POINT ( 'NONE',  ( 13.16986379960055054, -68.68124999999983515, -13.16986379959834430 ) ) ;
#17028 = CARTESIAN_POINT ( 'NONE',  ( 9.196399029521009183, 54.82142415364398147, -9.883404478874858512 ) ) ;
#17029 = CARTESIAN_POINT ( 'NONE',  ( 1.561832610794586538E-12, -54.11249999999986926, -18.62500000000000000 ) ) ;
#17030 = CARTESIAN_POINT ( 'NONE',  ( -5.326757387803152000, 65.48730266374865039, 12.40478207065405414 ) ) ;
#17031 = EDGE_CURVE ( 'NONE', #6792, #15852, #10427, .T. ) ;
#17032 = CARTESIAN_POINT ( 'NONE',  ( 5.883989548015876814, 30.92926152634062475, 10.19133431864935879 ) ) ;
#17033 = CARTESIAN_POINT ( 'NONE',  ( -7.404127077858561279, 35.40322001988060663, 11.28898901884024575 ) ) ;
#17034 = ORIENTED_EDGE ( 'NONE', *, *, #14149, .T. ) ;
#17035 = CARTESIAN_POINT ( 'NONE',  ( -13.49999999999999822, 9.079999999999996518, 4.386415899144235020 ) ) ;
#17036 = CARTESIAN_POINT ( 'NONE',  ( 5.441113646577305119, 5.918584287042172321, 25.42428528562857792 ) ) ;
#17037 = CARTESIAN_POINT ( 'NONE',  ( -11.39951685142248472, 32.20067605253005638, 7.232905375332705056 ) ) ;
#17038 = FACE_OUTER_BOUND ( 'NONE', #15921, .T. ) ;
#17039 = CARTESIAN_POINT ( 'NONE',  ( 10.54843083679575777, 60.10877045344361136, 8.425780205297863645 ) ) ;
#17040 = CARTESIAN_POINT ( 'NONE',  ( -8.549982208541774191E-16, -2.320000000000000728, 14.19474002721660355 ) ) ;
#17041 = DIRECTION ( 'NONE',  ( -0.000000000000000000, 1.000000000000000000, -0.000000000000000000 ) ) ;
#17042 = CARTESIAN_POINT ( 'NONE',  ( -7.272992578804310604, 60.37999999999998835, 10.01041549318726709 ) ) ;
#17043 = CARTESIAN_POINT ( 'NONE',  ( -13.49999999999999822, 72.77999999999998693, -4.386415899144240349 ) ) ;
#17044 = CARTESIAN_POINT ( 'NONE',  ( 13.48776120987618832, 51.44981947385706889, -0.5755966164107423344 ) ) ;
#17045 = CARTESIAN_POINT ( 'NONE',  ( -9.402578460527420745, 38.31120751014685055, 9.687247897747974790 ) ) ;
#17046 = CARTESIAN_POINT ( 'NONE',  ( 13.46426786292204092, 36.46463268930063606, -1.000909027039728949 ) ) ;
#17047 = CARTESIAN_POINT ( 'NONE',  ( -11.37500000000039613, -66.56562499999985505, 4.711679271993000739 ) ) ;
#17048 = CARTESIAN_POINT ( 'NONE',  ( -4.657935592016353432, 74.51210959751468010, 12.67423086677022859 ) ) ;
#17049 = DIRECTION ( 'NONE',  ( 1.000000000000000000, 1.734723475976807094E-16, 0.000000000000000000 ) ) ;
#17050 = EDGE_CURVE ( 'NONE', #1377, #13443, #13989, .T. ) ;
#17051 = CARTESIAN_POINT ( 'NONE',  ( 2.225286710710059790, 62.76010538675705419, 13.31609065531246117 ) ) ;
#17052 = CARTESIAN_POINT ( 'NONE',  ( 6.616676866212972294E-07, 41.68001839382905160, 13.49999999999996625 ) ) ;
#17053 = EDGE_LOOP ( 'NONE', ( #223, #11724, #12996, #10275, #16746, #9038, #12854, #1510 ) ) ;
#17054 = CARTESIAN_POINT ( 'NONE',  ( -11.76794919243112325, 15.78000000000001535, -3.823638476888998827 ) ) ;
#17055 = ORIENTED_EDGE ( 'NONE', *, *, #11541, .F. ) ;
#17056 = CARTESIAN_POINT ( 'NONE',  ( -9.520470885617717371, 57.23000000000000398, 6.917026985038133624 ) ) ;
#17057 = CARTESIAN_POINT ( 'NONE',  ( -11.37499999999960387, -7.284374999999982059, -4.711679271994910323 ) ) ;
#17058 = LINE ( 'NONE', #15545, #8767 ) ;
#17059 = CARTESIAN_POINT ( 'NONE',  ( -8.343458848123582072, 2.380000000000003002, 11.48378591275254124 ) ) ;
#17060 = CARTESIAN_POINT ( 'NONE',  ( 3.114363690246298333, 80.92999999999999261, -12.90281209101399718 ) ) ;
#17061 = CARTESIAN_POINT ( 'NONE',  ( 18.62499999999934985, -48.90937499999988347, 7.714727599200467800 ) ) ;
#17062 = CARTESIAN_POINT ( 'NONE',  ( -5.441113646577473872, 5.918584287042170544, -25.42428528562855305 ) ) ;
#17063 =( BOUNDED_CURVE ( )  B_SPLINE_CURVE ( 2, ( #2979, #4505, #2890, #12367, #4592, #4325, #3157 ),
 .UNSPECIFIED., .F., .F. ) 
 B_SPLINE_CURVE_WITH_KNOTS ( ( 3, 2, 2, 3 ),
 ( 0.6084947812034886550, 0.6113249933232189903, 0.6169854099280641657, 0.6212982611378772280 ),
 .UNSPECIFIED. ) 
 CURVE ( )  GEOMETRIC_REPRESENTATION_ITEM ( )  RATIONAL_B_SPLINE_CURVE ( ( 0.9755282581476212300, 0.9755282251407595417, 1.000000000000000000, 0.9510565162951535312, 1.000000000000000000, 0.9627084051148780963, 0.9822441115907478704 ) ) 
 REPRESENTATION_ITEM ( '' )  );
#17064 = CARTESIAN_POINT ( 'NONE',  ( 11.76794919243112680, 52.57999999999999119, -3.823638476888993942 ) ) ;
#17065 = CARTESIAN_POINT ( 'NONE',  ( 2.138192650046352394, 6.756881519606005249, 13.49999912087611165 ) ) ;
#17066 = CARTESIAN_POINT ( 'NONE',  ( -13.31562164696504702, 59.00890911105916103, 2.251771173006092308 ) ) ;
#17067 = CARTESIAN_POINT ( 'NONE',  ( 10.39222545102538930, 45.10021410930774977, 8.616954942238271187 ) ) ;
#17068 = CARTESIAN_POINT ( 'NONE',  ( 10.42247244000449236, 69.75827139048008974, -8.581908250913219405 ) ) ;
#17069 = CARTESIAN_POINT ( 'NONE',  ( 12.50000000000000000, 94.93000000000002103, 1.224646799147353059E-15 ) ) ;
#17070 = CARTESIAN_POINT ( 'NONE',  ( 13.41792843977121130, 30.37649222413373451, 1.532540479647116927 ) ) ;
#17071 = CARTESIAN_POINT ( 'NONE',  ( -6.645965699446401587, 55.42494999482337192, -11.75349136083715962 ) ) ;
#17072 = CARTESIAN_POINT ( 'NONE',  ( -10.88618976297357044, 50.23210744484570967, 7.983956116608660558 ) ) ;
#17073 = CARTESIAN_POINT ( 'NONE',  ( 2.002354034502180635, 64.10803839457231845, -13.35823153987989897 ) ) ;
#17074 = CARTESIAN_POINT ( 'NONE',  ( 2.930328270949149605, 43.07463622329592567, -13.17813713181922886 ) ) ;
#17075 = CARTESIAN_POINT ( 'NONE',  ( 13.31126723978048787, 39.35097732030541096, 2.249490025246444258 ) ) ;
#17076 = ORIENTED_EDGE ( 'NONE', *, *, #16042, .F. ) ;
#17077 = CARTESIAN_POINT ( 'NONE',  ( -9.857191988023737750, 70.57181382560094107, -9.224214792046671718 ) ) ;
#17078 = CARTESIAN_POINT ( 'NONE',  ( -10.17063788253329193, 61.58820356047785793, -8.877548349246254134 ) ) ;
#17079 = CARTESIAN_POINT ( 'NONE',  ( -9.520470885617717371, 4.230000000000011084, 6.917026985038133624 ) ) ;
#17080 = EDGE_LOOP ( 'NONE', ( #4850, #10144 ) ) ;
#17081 = CARTESIAN_POINT ( 'NONE',  ( -11.87325388569881923, 40.69222268659039798, -6.424704838537351748 ) ) ;
#17082 = EDGE_LOOP ( 'NONE', ( #3392, #3824, #14093, #5081 ) ) ;
#17083 = CARTESIAN_POINT ( 'NONE',  ( -4.171729424061787483, 31.32999999999999829, -12.83926296998457417 ) ) ;
#17084 = CARTESIAN_POINT ( 'NONE',  ( 18.62500000000000000, -16.64999999999995950, 1.560692158462880521E-12 ) ) ;
#17085 = CARTESIAN_POINT ( 'NONE',  ( 3.573871477204626057, 47.80835906961162607, 13.01915501523872898 ) ) ;
#17086 = CARTESIAN_POINT ( 'NONE',  ( 2.435209623814711399, 58.09243899615094620, -13.27854518587963994 ) ) ;
#17087 = CARTESIAN_POINT ( 'NONE',  ( 10.90896695675459327, 78.73074294728590417, -7.952685361619574067 ) ) ;
#17088 = CARTESIAN_POINT ( 'NONE',  ( -3.636496289402153081, 74.33000000000001251, -11.19198476289190936 ) ) ;
#17089 = CARTESIAN_POINT ( 'NONE',  ( 7.272992578804308828, 81.97999999999998977, 10.01041549318726709 ) ) ;
#17090 = DIRECTION ( 'NONE',  ( 0.000000000000000000, 0.000000000000000000, -1.000000000000000000 ) ) ;
#17091 = CARTESIAN_POINT ( 'NONE',  ( 10.92172942406178926, 41.13000000000000256, 7.935100905948387684 ) ) ;
#17092 = DIRECTION ( 'NONE',  ( -0.000000000000000000, 1.000000000000000000, -0.000000000000000000 ) ) ;
#17093 = CARTESIAN_POINT ( 'NONE',  ( -11.37500000000039790, -2.115624999999976996, 4.711679271993001628 ) ) ;
#17094 = DIRECTION ( 'NONE',  ( 0.000000000000000000, 0.000000000000000000, 1.000000000000000000 ) ) ;
#17095 = CARTESIAN_POINT ( 'NONE',  ( 7.992257996257984942, 33.87745199680230712, -10.88024195981830644 ) ) ;
#17096 = CARTESIAN_POINT ( 'NONE',  ( -13.35157257491907501, 73.86008181057655975, -1.996374706267173282 ) ) ;
#17097 = ORIENTED_EDGE ( 'NONE', *, *, #2626, .T. ) ;
#17098 = CARTESIAN_POINT ( 'NONE',  ( 27.07453251570901642, -7.999999999999996447, -22.50000000000000355 ) ) ;
#17099 = VERTEX_POINT ( 'NONE', #11275 ) ;
#17100 = CARTESIAN_POINT ( 'NONE',  ( 10.92172942406179104, 15.72999999999999332, -7.935100905948385908 ) ) ;
#17101 = CARTESIAN_POINT ( 'NONE',  ( -4.711679271993001628, -45.75312499999991189, -11.37500000000039613 ) ) ;
#17102 = CARTESIAN_POINT ( 'NONE',  ( 8.693978366012524717, 78.01462589808923553, 10.32788272577161592 ) ) ;
#17103 = CARTESIAN_POINT ( 'NONE',  ( -1.421462911354186565, 59.62892950574180873, 13.42717527354799678 ) ) ;
#17104 = FACE_BOUND ( 'NONE', #17080, .T. ) ;
#17105 = CARTESIAN_POINT ( 'NONE',  ( 7.500000000000001776, 88.93000000000000682, -12.00000000000000178 ) ) ;
#17106 = VECTOR ( 'NONE', #1931, 1000.000000000000000 ) ;
#17107 = CARTESIAN_POINT ( 'NONE',  ( 13.50000000000000000, 51.43000000000000682, 1.653273178848926867E-15 ) ) ;
#17108 = CARTESIAN_POINT ( 'NONE',  ( -2.115205434462649858, 71.60398018051243696, 13.34140295613403993 ) ) ;
#17109 = EDGE_CURVE ( 'NONE', #13215, #10472, #7563, .T. ) ;
#17110 = DIRECTION ( 'NONE',  ( -0.000000000000000000, 1.000000000000000000, -0.000000000000000000 ) ) ;
#17111 = CARTESIAN_POINT ( 'NONE',  ( -18.62500000000000000, -58.27499999999986358, -1.562973063126292555E-12 ) ) ;
#17112 = CARTESIAN_POINT ( 'NONE',  ( -4.336776230996957970, 68.52404150519048187, 12.78447647008732346 ) ) ;
#17113 = CARTESIAN_POINT ( 'NONE',  ( 18.62499999999934630, -65.55937499999984652, 7.714727599200467800 ) ) ;
#17114 = CARTESIAN_POINT ( 'NONE',  ( 3.266988135744673283, 55.06253129067860641, -13.09873820099263497 ) ) ;
#17115 = CARTESIAN_POINT ( 'NONE',  ( -1.564113515457998572E-12, -45.78749999999988773, 18.62500000000000000 ) ) ;
#17116 = VECTOR ( 'NONE', #10573, 1000.000000000000000 ) ;
#17117 = CARTESIAN_POINT ( 'NONE',  ( -10.08091572923360424, 65.27659544378147416, 8.982667173593638310 ) ) ;
#17118 = CARTESIAN_POINT ( 'NONE',  ( 12.00000000000000355, 8.446025403784434005, -3.899036354794874093 ) ) ;
#17119 = CARTESIAN_POINT ( 'NONE',  ( -4.481246075549229602, 35.51878334606949750, 12.73455671735402994 ) ) ;
#17120 = CARTESIAN_POINT ( 'NONE',  ( 4.171729424061791924, 23.02999999999999403, -12.83926296998457239 ) ) ;
#17121 = EDGE_LOOP ( 'NONE', ( #13658, #11964, #6968, #15566 ) ) ;
#17122 = FACE_OUTER_BOUND ( 'NONE', #7667, .T. ) ;
#17123 = LINE ( 'NONE', #14205, #977 ) ;
#17124 = CARTESIAN_POINT ( 'NONE',  ( -12.62330813568438792, 32.10339270682073476, 4.785626202566086285 ) ) ;
#17125 = DIRECTION ( 'NONE',  ( 0.000000000000000000, -0.000000000000000000, 1.000000000000000000 ) ) ;
#17126 = CARTESIAN_POINT ( 'NONE',  ( 13.49999999999999822, -10.72000000000000242, 4.386415899144237684 ) ) ;
#17127 = CARTESIAN_POINT ( 'NONE',  ( -7.077732738505361887, 53.41707563513180901, 11.49595236288632627 ) ) ;
#17128 = CARTESIAN_POINT ( 'NONE',  ( 7.272992578804308828, 57.97999999999999687, 10.01041549318726709 ) ) ;
#17129 = CARTESIAN_POINT ( 'NONE',  ( -13.49999999999999822, 75.78000000000000114, -4.386415899144240349 ) ) ;
#17130 = EDGE_CURVE ( 'NONE', #8781, #6383, #3681, .T. ) ;
#17131 = CARTESIAN_POINT ( 'NONE',  ( 12.69226882388820599, 51.59630501348791398, -4.600748021751061678 ) ) ;
#17132 = CARTESIAN_POINT ( 'NONE',  ( -13.34138775959904244, 38.00232289503568950, 2.063385629570992919 ) ) ;
#17133 = CARTESIAN_POINT ( 'NONE',  ( 11.91545564918995126, 36.66462542775949629, -6.346213808376679921 ) ) ;
#17134 = CARTESIAN_POINT ( 'NONE',  ( 4.711679271994911211, -76.97187499999985505, -11.37499999999960210 ) ) ;
#17135 = DIRECTION ( 'NONE',  ( -0.000000000000000000, 1.000000000000000000, -0.000000000000000000 ) ) ;
#17136 = CARTESIAN_POINT ( 'NONE',  ( -2.852822558295584177, 77.57736489273231939, 13.19697695634420320 ) ) ;
#17137 = CARTESIAN_POINT ( 'NONE',  ( -5.915749621473453068, 80.46455098764486991, 12.14391229634712843 ) ) ;
#17138 = APPLICATION_CONTEXT ( 'automotive_design' ) ;
#17139 = CARTESIAN_POINT ( 'NONE',  ( 12.50000000000000000, 98.93000000000002103, 1.224646799147353059E-15 ) ) ;
#17140 = VERTEX_POINT ( 'NONE', #16477 ) ;
#17141 = CARTESIAN_POINT ( 'NONE',  ( 3.636496289402154414, 13.83000000000000895, 11.19198476289190758 ) ) ;
#17142 = ORIENTED_EDGE ( 'NONE', *, *, #53, .T. ) ;
#17143 = CARTESIAN_POINT ( 'NONE',  ( 11.76794919243112680, 58.57999999999999119, -3.823638476888993942 ) ) ;
#17144 = CARTESIAN_POINT ( 'NONE',  ( -11.37500000000039790, -52.06562499999986926, 4.711679271993001628 ) ) ;
#17145 = CARTESIAN_POINT ( 'NONE',  ( -8.891200544363830713E-16, 55.67999999999999972, 13.50000000000000000 ) ) ;
#17146 = CARTESIAN_POINT ( 'NONE',  ( 4.171729424061789260, 2.829999999999999183, 12.83926296998457239 ) ) ;
#17147 = CARTESIAN_POINT ( 'NONE',  ( 12.08595287045816846, 75.65140306865309583, -6.015039302107231478 ) ) ;
#17148 = CARTESIAN_POINT ( 'NONE',  ( -1.564113515457998572E-12, -95.73749999999976978, 18.62500000000000000 ) ) ;
#17149 = CARTESIAN_POINT ( 'NONE',  ( 2.607531440858944223E-15, 70.17999999999997840, -14.19474002721660355 ) ) ;
#17150 = CARTESIAN_POINT ( 'NONE',  ( -11.76794919243112325, 39.07999999999999119, 3.823638476888994386 ) ) ;
#17151 = CARTESIAN_POINT ( 'NONE',  ( 12.50000000000000000, -18.00000000000000355, -9.000000000000001776 ) ) ;
#17152 = ADVANCED_FACE ( 'NONE', ( #4382 ), #9790, .F. ) ;
#17153 = CARTESIAN_POINT ( 'NONE',  ( -13.23010340770828819, 59.02482559903121029, 2.686282092327874516 ) ) ;
#17154 = CARTESIAN_POINT ( 'NONE',  ( 9.325152389469117509, 45.04492270333427939, 9.763112469116524750 ) ) ;
#17155 = CARTESIAN_POINT ( 'NONE',  ( 11.18517818444429146, 69.71422477896196312, -7.559393193918001685 ) ) ;
#17156 = CARTESIAN_POINT ( 'NONE',  ( 4.178864255851000829E-14, 67.68000000000000682, 13.50000000000000000 ) ) ;
#17157 = CARTESIAN_POINT ( 'NONE',  ( 12.40129267899110843, 30.23522311285729103, 5.337816854594090721 ) ) ;
#17158 = CARTESIAN_POINT ( 'NONE',  ( -10.96637117676712592, 55.63253460068611389, -7.873773472809477703 ) ) ;
#17159 = CARTESIAN_POINT ( 'NONE',  ( -13.45899139158765934, 49.96641258070299330, 1.051480819376249931 ) ) ;
#17160 = CARTESIAN_POINT ( 'NONE',  ( 7.778831186465364311, 63.88691009081542660, -11.03359887021824726 ) ) ;
#17161 = CARTESIAN_POINT ( 'NONE',  ( 5.971037608866275548, 42.96220972369073365, -12.10899681649361170 ) ) ;
#17162 = CARTESIAN_POINT ( 'NONE',  ( 12.51150814717434301, 39.24561605109204976, 5.070717436111691789 ) ) ;
#17163 = AXIS2_PLACEMENT_3D ( 'NONE', #10765, #14633, #12083 ) ;
#17164 = ORIENTED_EDGE ( 'NONE', *, *, #422, .F. ) ;
#17165 = DIRECTION ( 'NONE',  ( 0.000000000000000000, -1.000000000000000000, 0.000000000000000000 ) ) ;
#17166 = CARTESIAN_POINT ( 'NONE',  ( -5.323744072031061592, 70.37266774894109744, -12.40601925059792521 ) ) ;
#17167 = CARTESIAN_POINT ( 'NONE',  ( -11.07862474627882676, 61.63925496902839996, -7.715267273307309992 ) ) ;
#17168 = CARTESIAN_POINT ( 'NONE',  ( 11.76794919243112680, 5.580000000000004512, -3.823638476888993942 ) ) ;
#17169 = VERTEX_POINT ( 'NONE', #8465 ) ;
#17170 = CARTESIAN_POINT ( 'NONE',  ( -8.374905390823455420, 40.49983323364575938, -10.58857845316724955 ) ) ;
#17171 = ORIENTED_EDGE ( 'NONE', *, *, #10114, .T. ) ;
#17172 = CARTESIAN_POINT ( 'NONE',  ( 4.171729424061789260, 23.83000000000001961, 12.83926296998457239 ) ) ;
#17173 = CARTESIAN_POINT ( 'NONE',  ( 18.62499999999934630, -98.85937499999975842, 7.714727599200467800 ) ) ;
#17174 = CARTESIAN_POINT ( 'NONE',  ( 3.335671357901609735, 47.79992449767792095, 13.08141749487722372 ) ) ;
#17175 = CARTESIAN_POINT ( 'NONE',  ( 12.46660470777568186, 57.24137550530535634, 5.180132773053787609 ) ) ;
#17176 = CARTESIAN_POINT ( 'NONE',  ( 12.39391271687589757, 78.62543992849703045, -5.357776339167851454 ) ) ;
#17177 = CARTESIAN_POINT ( 'NONE',  ( -11.76794919243112325, 77.77999999999998693, -3.823638476888998827 ) ) ;
#17178 = CARTESIAN_POINT ( 'NONE',  ( -9.520470885617715595, 77.63000000000000966, -6.917026985038136289 ) ) ;
#17179 = CARTESIAN_POINT ( 'NONE',  ( -7.291143994141260196E-08, 47.67999796853253258, 13.49999999999999822 ) ) ;
#17180 = VECTOR ( 'NONE', #10011, 1000.000000000000000 ) ;
#17181 =( NAMED_UNIT ( * ) PLANE_ANGLE_UNIT ( ) SI_UNIT ( $, .RADIAN. ) );
#17182 = DIRECTION ( 'NONE',  ( 9.637352644315592778E-17, -1.000000000000000000, 0.000000000000000000 ) ) ;
#17183 = CARTESIAN_POINT ( 'NONE',  ( -11.37499999999960743, -83.28437499999976978, -4.711679271994912099 ) ) ;
#17184 = DIRECTION ( 'NONE',  ( -1.927470528863120035E-16, 1.000000000000000000, 0.000000000000000000 ) ) ;
#17185 = CARTESIAN_POINT ( 'NONE',  ( 3.313381788577463460, 34.06089591670649241, -13.08774833668259596 ) ) ;
#17186 = CARTESIAN_POINT ( 'NONE',  ( -5.778135341741982955, 73.39007587504690378, -12.20906592379313338 ) ) ;
#17187 = ORIENTED_EDGE ( 'NONE', *, *, #14173, .T. ) ;
#17188 = VERTEX_POINT ( 'NONE', #13817 ) ;
#17189 = CARTESIAN_POINT ( 'NONE',  ( 0.000000000000000000, 80.93000000000000682, 0.000000000000000000 ) ) ;
#17190 = ORIENTED_EDGE ( 'NONE', *, *, #15969, .F. ) ;
#17191 = CARTESIAN_POINT ( 'NONE',  ( 4.171729424061791924, 13.03000000000001357, -12.83926296998457239 ) ) ;
#17192 = CARTESIAN_POINT ( 'NONE',  ( -12.63745303140438025, 41.10210505988063545, 4.752538550325648536 ) ) ;
#17193 = CARTESIAN_POINT ( 'NONE',  ( 4.711679271994909435, -86.37187499999978968, -11.37499999999960387 ) ) ;
#17194 = CIRCLE ( 'NONE', #9036, 5.000000000000000000 ) ;
#17195 = ADVANCED_FACE ( 'NONE', ( #5809 ), #11192, .F. ) ;
#17196 = CARTESIAN_POINT ( 'NONE',  ( -3.792042785133936444, 44.54366267120555278, 12.96098082846388522 ) ) ;
#17197 = DIRECTION ( 'NONE',  ( -0.000000000000000000, 1.000000000000000000, -0.000000000000000000 ) ) ;
#17198 = CARTESIAN_POINT ( 'NONE',  ( 10.28586292936556035, 66.76562354563812107, -8.746356043348972875 ) ) ;
#17199 = CARTESIAN_POINT ( 'NONE',  ( 10.92172942406179104, 57.73000000000000398, -7.935100905948385908 ) ) ;
#17200 = CARTESIAN_POINT ( 'NONE',  ( -5.777759612418916113, 71.46979505895083662, 12.20112894437323448 ) ) ;
#17201 = CIRCLE ( 'NONE', #1950, 26.00000000000000355 ) ;
#17202 = CARTESIAN_POINT ( 'NONE',  ( -13.16986379960055409, -3.156249999999973355, 13.16986379959834252 ) ) ;
#17203 = CARTESIAN_POINT ( 'NONE',  ( -12.40275955986556511, 68.12471638559529197, 5.337660197801636031 ) ) ;
#17204 = CARTESIAN_POINT ( 'NONE',  ( 7.714727599200456254, -12.52187499999995524, -18.62499999999935341 ) ) ;
#17205 = CARTESIAN_POINT ( 'NONE',  ( -22.50000000000000355, -18.00000000000000711, -2.204364238465235822E-15 ) ) ;
#17206 = CARTESIAN_POINT ( 'NONE',  ( 7.714727599200458030, -69.72187499999982663, -18.62499999999934985 ) ) ;
#17207 = CARTESIAN_POINT ( 'NONE',  ( -11.48671059256369809, 65.19488865378939124, 7.092688608552144558 ) ) ;
#17208 = CARTESIAN_POINT ( 'NONE',  ( -2.138189944381236884, 42.25688142232025513, -13.50000000000000000 ) ) ;
#17209 = CARTESIAN_POINT ( 'NONE',  ( -7.122685775326801583, 35.41518282793498429, 11.46823613547876519 ) ) ;
#17210 = ORIENTED_EDGE ( 'NONE', *, *, #11185, .F. ) ;
#17211 = CARTESIAN_POINT ( 'NONE',  ( 7.999999999999849010, 0.000000000000000000, 24.73863375370601148 ) ) ;
#17212 = CARTESIAN_POINT ( 'NONE',  ( -13.35386423627540609, 31.99936814110893124, 1.981034437641194579 ) ) ;
#17213 = DIRECTION ( 'NONE',  ( 0.000000000000000000, 0.000000000000000000, 1.000000000000000000 ) ) ;
#17214 = CARTESIAN_POINT ( 'NONE',  ( 7.778968238013479031, 59.97315827432415603, 11.04249575341565226 ) ) ;
#17215 = CARTESIAN_POINT ( 'NONE',  ( 10.92172942406179104, -7.269999999999998685, -7.935100905948385908 ) ) ;
#17216 = CARTESIAN_POINT ( 'NONE',  ( -7.117030497825690638, 53.41541882487880599, 11.47162506946301264 ) ) ;
#17217 = CARTESIAN_POINT ( 'NONE',  ( 9.520470885617715595, 61.13000000000000256, 6.917026985038134512 ) ) ;
#17218 = APPLICATION_PROTOCOL_DEFINITION ( 'draft international standard', 'automotive_design', 1998, #556 ) ;
#17219 = CARTESIAN_POINT ( 'NONE',  ( -13.49999999999999822, 73.07999999999999829, 4.386415899144235908 ) ) ;
#17220 = CARTESIAN_POINT ( 'NONE',  ( 12.63394858448386060, 51.25764418862813443, 4.758328410953491350 ) ) ;
#17221 = CARTESIAN_POINT ( 'NONE',  ( -9.247281560364921660, 38.31892948853179348, 9.836254178153822636 ) ) ;
#17222 = CARTESIAN_POINT ( 'NONE',  ( 13.04399343315539284, 36.55404056568025339, -3.479124366659556600 ) ) ;
#17223 = CARTESIAN_POINT ( 'NONE',  ( 11.37499999999999645, -73.84999999999983800, 9.531744055041752924E-13 ) ) ;
#17224 = CARTESIAN_POINT ( 'NONE',  ( 7.416407864998737054, 1.846025403784438579, 10.20780970022447853 ) ) ;
#17225 = CARTESIAN_POINT ( 'NONE',  ( -12.14161640138082099, 77.14691383429233440, 5.901796293640162006 ) ) ;
#17226 = CARTESIAN_POINT ( 'NONE',  ( 2.042728443928158555, 62.75352127038405570, 13.34650732204479517 ) ) ;
#17227 = CARTESIAN_POINT ( 'NONE',  ( 7.500000000000000000, 107.2276959944580170, -6.931232109908920691 ) ) ;
#17228 = ORIENTED_EDGE ( 'NONE', *, *, #16241, .F. ) ;
#17229 = DIRECTION ( 'NONE',  ( 0.000000000000000000, -1.000000000000000000, 0.000000000000000000 ) ) ;
#17230 = CARTESIAN_POINT ( 'NONE',  ( 9.520470885617715595, 8.129999999999999005, 6.917026985038135400 ) ) ;
#17231 = EDGE_LOOP ( 'NONE', ( #5357, #2584, #17315, #12678 ) ) ;
#17232 = CARTESIAN_POINT ( 'NONE',  ( 3.636496289402154414, 54.83000000000000540, 11.19198476289190936 ) ) ;
#17233 = CARTESIAN_POINT ( 'NONE',  ( 8.043339635996302306, -90.56874999999976694, 8.043339635997654113 ) ) ;
#17234 = CARTESIAN_POINT ( 'NONE',  ( 10.92172942406179104, 56.73000000000000398, -7.935100905948385908 ) ) ;
#17235 = CARTESIAN_POINT ( 'NONE',  ( 8.343458848123578520, -6.020000000000000462, 11.48378591275254124 ) ) ;
#17236 = EDGE_CURVE ( 'NONE', #1976, #7754, #6236, .T. ) ;
#17237 = CARTESIAN_POINT ( 'NONE',  ( 10.55045400823578383, 75.75110043089878786, -8.422467017699190706 ) ) ;
#17238 = CARTESIAN_POINT ( 'NONE',  ( 13.49999999999999822, 68.28000000000000114, 4.386415899144236796 ) ) ;
#17239 = CARTESIAN_POINT ( 'NONE',  ( 13.50000000000000355, 69.58000000000001251, -4.386415899144233244 ) ) ;
#17240 = CARTESIAN_POINT ( 'NONE',  ( 7.272992578804311492, 37.87999999999999545, -10.01041549318726709 ) ) ;
#17241 = CARTESIAN_POINT ( 'NONE',  ( -1.732050807569007977, 7.773118517290099838, 18.99999999999998224 ) ) ;
#17242 = CARTESIAN_POINT ( 'NONE',  ( -13.44371064922030179, 58.97279030514989273, 1.233250831257197921 ) ) ;
#17243 = CARTESIAN_POINT ( 'NONE',  ( 8.616471885361647765, 45.01100696542791013, 10.39501578887478850 ) ) ;
#17244 = CARTESIAN_POINT ( 'NONE',  ( 11.96655270214789546, 69.66073437090237519, -6.249154475983210943 ) ) ;
#17245 = CARTESIAN_POINT ( 'NONE',  ( -13.50000000000000000, 66.93000000000000682, -3.306546357697853733E-15 ) ) ;
#17246 = CARTESIAN_POINT ( 'NONE',  ( -12.10101126829370877, 55.70980494182975917, -5.984645542856269707 ) ) ;
#17247 = CARTESIAN_POINT ( 'NONE',  ( -12.46869863188028127, 50.11846721888420575, 5.176712836207804536 ) ) ;
#17248 = CARTESIAN_POINT ( 'NONE',  ( 2.777601260996298560, 64.08012766020287643, -13.21117397333636845 ) ) ;
#17249 = CARTESIAN_POINT ( 'NONE',  ( 10.24342786741839895, 42.76787029749926461, -8.793327985299702831 ) ) ;
#17250 = CARTESIAN_POINT ( 'NONE',  ( 12.62628274794963268, 39.25686581151648369, 4.778813820910057686 ) ) ;
#17251 = ORIENTED_EDGE ( 'NONE', *, *, #1152, .F. ) ;
#17252 = CARTESIAN_POINT ( 'NONE',  ( -5.269151658466837418, 70.37058849064762001, -12.42925709556887348 ) ) ;
#17253 = CARTESIAN_POINT ( 'NONE',  ( -11.76356277521508353, 61.68370007369408370, -6.634314378474659435 ) ) ;
#17254 = CARTESIAN_POINT ( 'NONE',  ( -7.272992578804310604, 7.380000000000005222, 10.01041549318726709 ) ) ;
#17255 = VERTEX_POINT ( 'NONE', #4732 ) ;
#17256 = EDGE_CURVE ( 'NONE', #5186, #7488, #2673, .T. ) ;
#17257 = VERTEX_POINT ( 'NONE', #9768 ) ;
#17258 = CARTESIAN_POINT ( 'NONE',  ( 10.92172942406178926, 21.13000000000000966, 7.935100905948385908 ) ) ;
#17259 = CARTESIAN_POINT ( 'NONE',  ( 18.62500000000064304, -67.64062499999984368, -7.714727599197335195 ) ) ;
#17260 = CARTESIAN_POINT ( 'NONE',  ( 3.023893711184864497, 61.07127210962161712, -13.15699171173593562 ) ) ;
#17261 = CARTESIAN_POINT ( 'NONE',  ( 13.46692166222190323, 57.46359382206249222, -0.9738314228308512233 ) ) ;
#17262 = CARTESIAN_POINT ( 'NONE',  ( 11.76794919243112325, 73.42999999999999261, 1.441158131103945434E-15 ) ) ;
#17263 = CARTESIAN_POINT ( 'NONE',  ( -4.171729424061791036, 37.53000000000000114, 12.83926296998457239 ) ) ;
#17264 = CARTESIAN_POINT ( 'NONE',  ( 11.76794919243112325, 79.43000000000000682, 1.441158131103945434E-15 ) ) ;
#17265 = CARTESIAN_POINT ( 'NONE',  ( 2.894739590358088936E-06, 0.6800804143413337055, 13.49999999999938360 ) ) ;
#17266 = CARTESIAN_POINT ( 'NONE',  ( 4.722607142260388358, -99.99999999999995737, 12.69610481275498870 ) ) ;
#17267 = CARTESIAN_POINT ( 'NONE',  ( 1.204171936209234461, 9.999999999999996447, -13.21877505270804143 ) ) ;
#17268 = CARTESIAN_POINT ( 'NONE',  ( -4.711679271994916540, -28.09687499999992966, 11.37499999999960210 ) ) ;
#17269 = CARTESIAN_POINT ( 'NONE',  ( -8.224360503536546367E-15, 78.17999999999999261, -13.50000000000000000 ) ) ;
#17270 = CARTESIAN_POINT ( 'NONE',  ( 4.705958961061473822, 34.01056731324530347, -12.65510421492889392 ) ) ;
#17271 = CARTESIAN_POINT ( 'NONE',  ( -10.48340775277034709, 73.60523400273746120, -8.505871817968104764 ) ) ;
#17272 = ORIENTED_EDGE ( 'NONE', *, *, #5760, .T. ) ;
#17273 = ORIENTED_EDGE ( 'NONE', *, *, #3986, .F. ) ;
#17274 = CARTESIAN_POINT ( 'NONE',  ( 11.76794919243112325, 79.43000000000000682, 1.441158131103945434E-15 ) ) ;
#17275 = VERTEX_POINT ( 'NONE', #7279 ) ;
#17276 = AXIS2_PLACEMENT_3D ( 'NONE', #32, #1010, #6421 ) ;
#17277 = EDGE_CURVE ( 'NONE', #8869, #13655, #3285, .T. ) ;
#17278 = CARTESIAN_POINT ( 'NONE',  ( -11.37500000000039613, -66.56562499999985505, 4.711679271993000739 ) ) ;
#17279 = CARTESIAN_POINT ( 'NONE',  ( -10.04614863194917085, 44.27837129718821529, 9.018666547317595317 ) ) ;
#17280 = CARTESIAN_POINT ( 'NONE',  ( -7.499999999999996447, -23.27245777243039271, 9.199283337799348814 ) ) ;
#17281 = CARTESIAN_POINT ( 'NONE',  ( 10.96346797855937005, 66.72754922618597107, -7.889439196751125927 ) ) ;
#17282 = CARTESIAN_POINT ( 'NONE',  ( 4.171729424061789260, 44.82999999999999829, 12.83926296998457417 ) ) ;
#17283 = CARTESIAN_POINT ( 'NONE',  ( -4.443453434118055156, 71.52016342193364551, 12.74779440899964911 ) ) ;
#17284 = VECTOR ( 'NONE', #2847, 1000.000000000000000 ) ;
#17285 = CARTESIAN_POINT ( 'NONE',  ( 7.714727599197338748, -63.47812499999984226, 18.62500000000063949 ) ) ;
#17286 = EDGE_CURVE ( 'NONE', #12239, #12048, #15466, .T. ) ;
#17287 = CARTESIAN_POINT ( 'NONE',  ( -11.67555045867362828, 68.18203702761856277, 6.777281805934028291 ) ) ;
#17288 = CARTESIAN_POINT ( 'NONE',  ( -18.62500000000000000, -91.57499999999977547, -1.562973063126292555E-12 ) ) ;
#17289 = CARTESIAN_POINT ( 'NONE',  ( 3.234907857666803999, 55.06368519065139111, -13.10671587365533952 ) ) ;
#17290 = CARTESIAN_POINT ( 'NONE',  ( -18.62500000000000000, -74.92499999999982663, -1.562973063126292555E-12 ) ) ;
#17291 = CARTESIAN_POINT ( 'NONE',  ( -11.56667719001696426, 65.18964896454224345, 6.962137039653539361 ) ) ;
#17292 = CARTESIAN_POINT ( 'NONE',  ( 1.708800344670653191E-06, 35.68004753840243382, 13.49999999999978328 ) ) ;
#17293 = CARTESIAN_POINT ( 'NONE',  ( 4.171729424061789260, 18.83000000000001251, 12.83926296998457239 ) ) ;
#17294 = ORIENTED_EDGE ( 'NONE', *, *, #2487, .F. ) ;
#17295 = CARTESIAN_POINT ( 'NONE',  ( 0.000000000000000000, 9.000000000000000000, 0.000000000000000000 ) ) ;
#17296 = CARTESIAN_POINT ( 'NONE',  ( -11.76794919243112325, 27.93000000000001037, -2.602085213965210642E-15 ) ) ;
#17297 = CARTESIAN_POINT ( 'NONE',  ( -4.031777158982798426, 31.32496779636636930, -12.88399759500174646 ) ) ;
#17298 = CARTESIAN_POINT ( 'NONE',  ( 0.9395320564595106561, 73.14622125165477939, -13.47038777558300104 ) ) ;
#17299 = CARTESIAN_POINT ( 'NONE',  ( -11.76794919243112325, -11.06999999999999673, -2.602085213965210642E-15 ) ) ;
#17300 = CARTESIAN_POINT ( 'NONE',  ( 6.717037858009446971, 59.92796916074577496, 11.71054420305484456 ) ) ;
#17301 = CARTESIAN_POINT ( 'NONE',  ( -8.549982208541774191E-16, -8.320000000000009166, 14.19474002721660355 ) ) ;
#17302 = CARTESIAN_POINT ( 'NONE',  ( -10.70683009229711580, 53.24250546810384321, 8.226716998541878212 ) ) ;
#17303 = CARTESIAN_POINT ( 'NONE',  ( -3.636496289402153081, 59.32999999999999829, -11.19198476289190936 ) ) ;
#17304 = APPLICATION_PROTOCOL_DEFINITION ( 'draft international standard', 'automotive_design', 1998, #16226 ) ;
#17305 = CARTESIAN_POINT ( 'NONE',  ( 13.50000000000000000, 71.43000000000000682, 1.653273178848926867E-15 ) ) ;
#17306 = CARTESIAN_POINT ( 'NONE',  ( 4.026175869006643815, 50.82453816887448284, 12.88888496101055203 ) ) ;
#17307 = CARTESIAN_POINT ( 'NONE',  ( -11.84723349959135419, 37.69029764867568133, -6.472542598240520029 ) ) ;
#17308 = CARTESIAN_POINT ( 'NONE',  ( 12.78455863521889846, 36.27369161258553731, 4.342181555957650652 ) ) ;
#17309 = CARTESIAN_POINT ( 'NONE',  ( -8.043339635996300530, -30.14374999999994742, -8.043339635997652337 ) ) ;
#17310 = CARTESIAN_POINT ( 'NONE',  ( 9.708203932499369415, 1.996025403784430496, 7.053423027509680310 ) ) ;
#17311 = CARTESIAN_POINT ( 'NONE',  ( -3.718240652620805164, 77.54630559155440039, 12.97798887002702628 ) ) ;
#17312 = CARTESIAN_POINT ( 'NONE',  ( -8.931564203448942862, 79.52510900431931873, -10.16074476288992834 ) ) ;
#17313 = CARTESIAN_POINT ( 'NONE',  ( 11.76794919243112325, 11.42999999999999616, 1.734723475976807094E-15 ) ) ;
#17314 = CARTESIAN_POINT ( 'NONE',  ( 7.500000000000002665, 108.7397976749055033, 0.4943161440816180030 ) ) ;
#17315 = ORIENTED_EDGE ( 'NONE', *, *, #12372, .T. ) ;
#17316 = LINE ( 'NONE', #2450, #2966 ) ;
#17317 = CARTESIAN_POINT ( 'NONE',  ( -7.272992578804310604, 7.380000000000005222, 10.01041549318726709 ) ) ;
#17318 = VERTEX_POINT ( 'NONE', #16978 ) ;
#17319 = CARTESIAN_POINT ( 'NONE',  ( -3.636496289402153081, 53.33000000000000540, -11.19198476289190936 ) ) ;
#17320 = CARTESIAN_POINT ( 'NONE',  ( 11.37499999999960565, -58.30937499999983231, 4.711679271994918317 ) ) ;
#17321 = CARTESIAN_POINT ( 'NONE',  ( 4.171729424061789260, 9.830000000000005400, 12.83926296998457239 ) ) ;
#17322 = CARTESIAN_POINT ( 'NONE',  ( 13.50000000000000000, -8.569999999999994955, 1.734723475976807094E-15 ) ) ;
#17323 = CARTESIAN_POINT ( 'NONE',  ( 11.35955556442647563, 75.70303036091502236, -7.298446421436677767 ) ) ;
#17324 = CARTESIAN_POINT ( 'NONE',  ( 13.49999999999999822, 32.27999999999999403, 4.386415899144236796 ) ) ;
#17325 = CARTESIAN_POINT ( 'NONE',  ( 8.343458848123578520, 74.98000000000000398, 11.48378591275254124 ) ) ;
#17326 = CARTESIAN_POINT ( 'NONE',  ( 3.636496289402157078, 41.02999999999999403, -11.19198476289190936 ) ) ;
#17327 = DIRECTION ( 'NONE',  ( 0.000000000000000000, -1.000000000000000000, 0.000000000000000000 ) ) ;
#17328 = CARTESIAN_POINT ( 'NONE',  ( -12.79740114811030871, 58.77520009425771974, -4.298488401906374712 ) ) ;
#17329 = EDGE_CURVE ( 'NONE', #15915, #5802, #10712, .T. ) ;
#17330 = CARTESIAN_POINT ( 'NONE',  ( 2.445080149700053643E-15, 36.17999999999999972, -13.50000000000000000 ) ) ;
#17331 = CARTESIAN_POINT ( 'NONE',  ( 11.94949547157306569, 69.66203931647574166, -6.281685575819165201 ) ) ;
#17332 = CARTESIAN_POINT ( 'NONE',  ( 17.32050807568878170, 0.000000000000000000, -7.999999999999961808 ) ) ;
#17333 = CARTESIAN_POINT ( 'NONE',  ( -3.708203932499366751, 3.463974596215561697, -11.41267819554184371 ) ) ;
#17334 = CARTESIAN_POINT ( 'NONE',  ( -5.804494891024957859, 55.39114009213712819, -12.19755537893474795 ) ) ;
#17335 = CARTESIAN_POINT ( 'NONE',  ( -8.882628454602302881, 50.33650084750680520, 10.16724425321487502 ) ) ;
#17336 = CARTESIAN_POINT ( 'NONE',  ( 13.48315231035429562, 63.40657019742398859, 0.6764558583580484452 ) ) ;
#17337 = CARTESIAN_POINT ( 'NONE',  ( 11.92691999087596422, 42.66375240387029066, -6.324443746775120445 ) ) ;
#17338 = CARTESIAN_POINT ( 'NONE',  ( 9.365081934501255034, 39.04690919444636421, 9.723838687483500109 ) ) ;
#17339 = VERTEX_POINT ( 'NONE', #2034 ) ;
#17340 = CARTESIAN_POINT ( 'NONE',  ( -12.75389532800142156, 70.77035997815164592, -4.425893360476143457 ) ) ;
#17341 = CARTESIAN_POINT ( 'NONE',  ( -6.678963197138114261, 61.42630604540634209, -11.73467470017203951 ) ) ;
#17342 = CARTESIAN_POINT ( 'NONE',  ( -9.520470885617717371, 1.230000000000008864, 6.917026985038133624 ) ) ;
#17343 = ORIENTED_EDGE ( 'NONE', *, *, #8049, .T. ) ;
#17344 = VECTOR ( 'NONE', #17448, 1000.000000000000000 ) ;
#17345 = ORIENTED_EDGE ( 'NONE', *, *, #160, .F. ) ;
#17346 = CARTESIAN_POINT ( 'NONE',  ( -4.171729424061791036, 20.53000000000001890, 12.83926296998457239 ) ) ;
#17347 = CARTESIAN_POINT ( 'NONE',  ( -13.16986379959834252, -89.49374999999979252, -13.16986379960055054 ) ) ;
#17348 = CARTESIAN_POINT ( 'NONE',  ( 4.350118814684195812, 61.02343481574471440, -12.78180230389262206 ) ) ;
#17349 = CARTESIAN_POINT ( 'NONE',  ( 8.343458848123578520, 9.979999999999996874, 11.48378591275254124 ) ) ;
#17350 = CARTESIAN_POINT ( 'NONE',  ( 6.655659527147368415, 71.92472051196341454, 11.77853259824717469 ) ) ;
#17351 = CARTESIAN_POINT ( 'NONE',  ( 12.97075051976666593, 57.29464339237642889, 3.781696856989037681 ) ) ;
#17352 = CARTESIAN_POINT ( 'NONE',  ( 3.636496289402157078, 71.03000000000000114, -11.19198476289190936 ) ) ;
#17353 = CARTESIAN_POINT ( 'NONE',  ( -7.272992578804307939, 74.47999999999998977, -10.01041549318726886 ) ) ;
#17354 = CARTESIAN_POINT ( 'NONE',  ( -6.109861361309374850, 47.45672596454227232, 12.04552982495143887 ) ) ;
#17355 = EDGE_CURVE ( 'NONE', #7272, #7126, #15232, .T. ) ;
#17356 = CARTESIAN_POINT ( 'NONE',  ( 11.14820950268467392, -99.99999999999997158, 13.72570587197042791 ) ) ;
#17357 = CARTESIAN_POINT ( 'NONE',  ( -8.343458848123582072, 76.37999999999998124, 11.48378591275253768 ) ) ;
#17358 = CARTESIAN_POINT ( 'NONE',  ( 4.711679271993006957, -89.52812499999977547, 11.37500000000039613 ) ) ;
#17359 = CARTESIAN_POINT ( 'NONE',  ( 0.000000000000000000, 0.000000000000000000, 0.000000000000000000 ) ) ;
#17360 = CARTESIAN_POINT ( 'NONE',  ( 13.16872902743496176, 33.53572654962647448, -2.983947442641389447 ) ) ;
#17361 = CARTESIAN_POINT ( 'NONE',  ( -2.284765042927564327, 73.26215171443423912, -13.30525723312327102 ) ) ;
#17362 = ORIENTED_EDGE ( 'NONE', *, *, #13247, .T. ) ;
#17363 = ORIENTED_EDGE ( 'NONE', *, *, #14149, .F. ) ;
#17364 = CARTESIAN_POINT ( 'NONE',  ( 11.76794919243112680, 79.57999999999999829, -3.823638476888993942 ) ) ;
#17365 = EDGE_LOOP ( 'NONE', ( #9670, #2517, #8889, #3390 ) ) ;
#17366 = CARTESIAN_POINT ( 'NONE',  ( -13.18318444668010159, 41.03483660876138117, 2.959365213291953012 ) ) ;
#17367 = CARTESIAN_POINT ( 'NONE',  ( 4.711679271994911211, -76.97187499999985505, -11.37499999999960210 ) ) ;
#17368 = CARTESIAN_POINT ( 'NONE',  ( -10.12576673064770461, 44.27415152351466077, 8.928542170256765331 ) ) ;
#17369 = CARTESIAN_POINT ( 'NONE',  ( -7.499999999999997335, -23.02061778433118278, 9.262340467025644841 ) ) ;
#17370 = CARTESIAN_POINT ( 'NONE',  ( -13.49999999999999822, 43.78000000000000114, -4.386415899144240349 ) ) ;
#17371 = CARTESIAN_POINT ( 'NONE',  ( -4.111532903675451323, 71.53223907380960611, 12.85981808316648234 ) ) ;
#17372 = AXIS2_PLACEMENT_3D ( 'NONE', #16930, #4833, #12961 ) ;
#17373 = ADVANCED_FACE ( 'NONE', ( #4880 ), #7370, .F. ) ;
#17374 = CARTESIAN_POINT ( 'NONE',  ( 13.16986379959833897, -7.318749999999964118, 13.16986379960055409 ) ) ;
#17375 = CARTESIAN_POINT ( 'NONE',  ( -12.91567691309717425, 67.78913409428740522, -3.929411082883120354 ) ) ;
#17376 = CARTESIAN_POINT ( 'NONE',  ( 13.16986379959834075, -97.81874999999976694, 13.16986379960055231 ) ) ;
#17377 = CARTESIAN_POINT ( 'NONE',  ( 4.917110454403338160, 55.00272141760193279, -12.57281145620107843 ) ) ;
#17378 = CARTESIAN_POINT ( 'NONE',  ( 0.000000000000000000, 73.00000000000001421, -5.000000000000000000 ) ) ;
#17379 = CARTESIAN_POINT ( 'NONE',  ( -13.46462703413381057, 64.89617492903833806, -0.9768049181541919035 ) ) ;
#17380 = CARTESIAN_POINT ( 'NONE',  ( -9.422069060292017184, 35.31024417702938933, 9.668260009429062052 ) ) ;
#17381 = ORIENTED_EDGE ( 'NONE', *, *, #3600, .F. ) ;
#17382 = DIRECTION ( 'NONE',  ( 1.000000000000000000, 0.000000000000000000, 0.000000000000000000 ) ) ;
#17383 = AXIS2_PLACEMENT_3D ( 'NONE', #2640, #3987, #9662 ) ;
#17384 = CARTESIAN_POINT ( 'NONE',  ( -4.450278236855409908, 31.34009545450314960, -12.74587338740473008 ) ) ;
#17385 = CYLINDRICAL_SURFACE ( 'NONE', #4569, 26.00000000000000355 ) ;
#17386 = CARTESIAN_POINT ( 'NONE',  ( 3.636496289402157078, -8.969999999999998863, -11.19198476289190936 ) ) ;
#17387 = CARTESIAN_POINT ( 'NONE',  ( 2.239639182115807703, 59.76050779538447699, 13.32172022568457059 ) ) ;
#17388 = CARTESIAN_POINT ( 'NONE',  ( 10.92172942406179104, -4.269999999999996021, -7.935100905948385908 ) ) ;
#17389 = CARTESIAN_POINT ( 'NONE',  ( -3.590842839537486952, 53.55089504792430688, 13.01397566794303984 ) ) ;
#17390 = CARTESIAN_POINT ( 'NONE',  ( -9.520470885617715595, 50.62999999999999545, -6.917026985038136289 ) ) ;
#17391 = CARTESIAN_POINT ( 'NONE',  ( -4.171729424061787483, 66.32999999999999829, -12.83926296998457417 ) ) ;
#17392 = CARTESIAN_POINT ( 'NONE',  ( 8.130178193921372198, 50.98872557350986057, 10.77736799249517397 ) ) ;
#17393 = CARTESIAN_POINT ( 'NONE',  ( -8.682891546362668578, 37.51407913491349433, -10.33829868067962465 ) ) ;
#17394 = CARTESIAN_POINT ( 'NONE',  ( 13.50091882085834349, 36.43068900341727812, -0.02411123018305068311 ) ) ;
#17395 = CARTESIAN_POINT ( 'NONE',  ( -11.37499999999999645, -82.17499999999982663, -9.545674412382054647E-13 ) ) ;
#17396 = CARTESIAN_POINT ( 'NONE',  ( -19.29752010712827826, 0.000000000000000000, -17.42428528562878398 ) ) ;
#17397 = CARTESIAN_POINT ( 'NONE',  ( -11.19998009217254342, 76.64669584381921652, -7.537276725262922916 ) ) ;
#17398 = CARTESIAN_POINT ( 'NONE',  ( -11.46985824616760929, 79.66346450398999934, -7.133603377940076484 ) ) ;
#17399 = CARTESIAN_POINT ( 'NONE',  ( 3.636496289402154414, 10.83000000000000540, 11.19198476289190758 ) ) ;
#17400 = CARTESIAN_POINT ( 'NONE',  ( 2.138189944381283514, 5.103118577679734535, -13.49999999999998401 ) ) ;
#17401 = CARTESIAN_POINT ( 'NONE',  ( 11.76794919243112325, 5.430000000000004157, 1.734723475976807094E-15 ) ) ;
#17402 = CARTESIAN_POINT ( 'NONE',  ( -3.636496289402155746, 51.53000000000000114, 11.19198476289190936 ) ) ;
#17403 = CARTESIAN_POINT ( 'NONE',  ( -8.043339635996304082, -82.24374999999977831, -8.043339635997652337 ) ) ;
#17404 = CARTESIAN_POINT ( 'NONE',  ( 18.62500000000064304, -34.34062499999991047, -7.714727599197335195 ) ) ;
#17405 = CARTESIAN_POINT ( 'NONE',  ( -4.171729424061787483, -4.669999999999993712, -12.83926296998457417 ) ) ;
#17406 = DIRECTION ( 'NONE',  ( 0.000000000000000000, 1.000000000000000000, 0.000000000000000000 ) ) ;
#17407 = CARTESIAN_POINT ( 'NONE',  ( 12.06866609241714805, 75.65277784651085824, -6.049575060431308771 ) ) ;
#17408 = EDGE_CURVE ( 'NONE', #10383, #9328, #636, .T. ) ;
#17409 = CARTESIAN_POINT ( 'NONE',  ( -7.499999999999992895, 88.93000000000000682, 9.367496997597603681 ) ) ;
#17410 = CARTESIAN_POINT ( 'NONE',  ( -11.76794919243112325, 44.77999999999998693, -3.823638476888998827 ) ) ;
#17411 = CARTESIAN_POINT ( 'NONE',  ( -4.310585880099474743, 41.52499022814427576, 12.79332601979654527 ) ) ;
#17412 = CARTESIAN_POINT ( 'NONE',  ( -7.240455008785836810, 58.44980870328423350, -11.40403264383034809 ) ) ;
#17413 = CARTESIAN_POINT ( 'NONE',  ( 2.809647516641907039, 44.78102113769125481, 13.20454587893587473 ) ) ;
#17414 = CARTESIAN_POINT ( 'NONE',  ( -2.138189944381236884, 54.25688142232026223, -13.50000000000000000 ) ) ;
#17415 = CARTESIAN_POINT ( 'NONE',  ( 2.222800136090958861E-15, 3.313974596215566670, -12.00000000000000355 ) ) ;
#17416 = CARTESIAN_POINT ( 'NONE',  ( -4.127767022055135016, 55.32841944913306520, -12.85353179314369676 ) ) ;
#17417 = CARTESIAN_POINT ( 'NONE',  ( -13.34267872512751829, 49.85780686539629869, -2.060371127682625758 ) ) ;
#17418 = CARTESIAN_POINT ( 'NONE',  ( 11.65055789732274683, 63.68395381943928157, -6.822091475785055259 ) ) ;
#17419 = CARTESIAN_POINT ( 'NONE',  ( 11.17912042028613939, 42.71459578989527728, -7.568175797576554231 ) ) ;
#17420 = CARTESIAN_POINT ( 'NONE',  ( 12.54038525704221918, 39.24839084401543232, 4.998944329035393430 ) ) ;
#17421 = ORIENTED_EDGE ( 'NONE', *, *, #14015, .F. ) ;
#17422 = CARTESIAN_POINT ( 'NONE',  ( -13.34284440902900926, 70.85780192660213572, -2.059723299679095287 ) ) ;
#17423 = CARTESIAN_POINT ( 'NONE',  ( -2.114379580585429075, 61.25589748944436508, -13.34258779510372683 ) ) ;
#17424 = ORIENTED_EDGE ( 'NONE', *, *, #15044, .T. ) ;
#17425 = EDGE_LOOP ( 'NONE', ( #11189, #4980, #996, #2477 ) ) ;
#17426 = CARTESIAN_POINT ( 'NONE',  ( -10.92172942406178926, 22.63000000000000966, -7.935100905948389460 ) ) ;
#17427 = CARTESIAN_POINT ( 'NONE',  ( 18.62500000000064304, -50.99062499999987352, -7.714727599197335195 ) ) ;
#17428 = ADVANCED_FACE ( 'NONE', ( #16802 ), #9196, .T. ) ;
#17429 = CARTESIAN_POINT ( 'NONE',  ( 4.771570364578763268, 61.00810182393892944, -12.62862348470532403 ) ) ;
#17430 = CARTESIAN_POINT ( 'NONE',  ( -10.92172942406179104, 12.23000000000000398, 7.935100905948385908 ) ) ;
#17431 = CARTESIAN_POINT ( 'NONE',  ( 1.941764556727805902, 71.74984903881171761, 13.36122291574299048 ) ) ;
#17432 = CARTESIAN_POINT ( 'NONE',  ( 13.28561249400892486, 57.51485447208779078, -2.406641530742766211 ) ) ;
#17433 = CARTESIAN_POINT ( 'NONE',  ( 3.636496289402157078, 65.03000000000000114, -11.19198476289190936 ) ) ;
#17434 = CARTESIAN_POINT ( 'NONE',  ( -3.636496289402153081, 80.32999999999999829, -11.19198476289190936 ) ) ;
#17435 = CARTESIAN_POINT ( 'NONE',  ( -2.129512067614891979, 47.60350643943056070, 13.33988058347349437 ) ) ;
#17436 = CARTESIAN_POINT ( 'NONE',  ( 1.653273178848926472E-15, 80.93000000000000682, 13.50000000000000000 ) ) ;
#17437 = CARTESIAN_POINT ( 'NONE',  ( 9.226448456246030716, -99.99999999999998579, 14.69264636604441776 ) ) ;
#17438 = CARTESIAN_POINT ( 'NONE',  ( -2.138189944381236884, 33.25688142232026934, -13.50000000000000000 ) ) ;
#17439 = CARTESIAN_POINT ( 'NONE',  ( 11.37499999999960565, -74.95937499999980957, 4.711679271994918317 ) ) ;
#17440 = CARTESIAN_POINT ( 'NONE',  ( 13.50000000000000000, 44.42999999999999972, 1.653273178848926867E-15 ) ) ;
#17441 = CARTESIAN_POINT ( 'NONE',  ( 13.03313334573954663, 33.55554678071828789, -3.519655650307517369 ) ) ;
#17442 = CARTESIAN_POINT ( 'NONE',  ( -9.170396273949972255, 73.53708420928282408, -9.917996326314725053 ) ) ;
#17443 = VERTEX_POINT ( 'NONE', #2813 ) ;
#17444 = EDGE_LOOP ( 'NONE', ( #13962, #3907 ) ) ;
#17445 = CARTESIAN_POINT ( 'NONE',  ( 7.272992578804308828, 72.98000000000000398, 10.01041549318726886 ) ) ;
#17446 = ORIENTED_EDGE ( 'NONE', *, *, #10666, .T. ) ;
#17447 = CARTESIAN_POINT ( 'NONE',  ( 13.16986379960055409, -9.331249999999993605, -13.16986379959834430 ) ) ;
#17448 = DIRECTION ( 'NONE',  ( 0.000000000000000000, -1.000000000000000000, 0.000000000000000000 ) ) ;
#17449 = EDGE_CURVE ( 'NONE', #6383, #2386, #4428, .T. ) ;
#17450 = CARTESIAN_POINT ( 'NONE',  ( -7.499999999999995559, -25.82163707610022740, -7.534909587719540447 ) ) ;
#17451 = VECTOR ( 'NONE', #3602, 1000.000000000000227 ) ;
#17452 = CARTESIAN_POINT ( 'NONE',  ( 2.607531440858944223E-15, 40.17999999999999972, -14.19474002721660355 ) ) ;
#17453 = CARTESIAN_POINT ( 'NONE',  ( -13.41700927251858566, 70.98327095921497687, 1.530665322069840517 ) ) ;
#17454 = CARTESIAN_POINT ( 'NONE',  ( -1.564113515457998370E-12, -21.88749999999992824, 18.62500000000000000 ) ) ;
#17455 = CARTESIAN_POINT ( 'NONE',  ( -13.35242449763338612, 67.99999608817336139, 1.998305130635517735 ) ) ;
#17456 = CARTESIAN_POINT ( 'NONE',  ( -18.62499999999934985, -90.53437499999978400, -7.714727599200458918 ) ) ;
#17457 = CARTESIAN_POINT ( 'NONE',  ( 12.04472249175536014, 54.65529430329254978, -6.116930152733188741 ) ) ;
#17458 = AXIS2_PLACEMENT_3D ( 'NONE', #9362, #10593, #7857 ) ;
#17459 = CARTESIAN_POINT ( 'NONE',  ( 3.636496289402154414, 19.83000000000001251, 11.19198476289190758 ) ) ;
#17460 = CARTESIAN_POINT ( 'NONE',  ( -7.714727599197335195, -71.80312499999982379, -18.62500000000064304 ) ) ;
#17461 = CARTESIAN_POINT ( 'NONE',  ( -11.63660655936212507, 65.18491705363410915, 6.845780105586399600 ) ) ;
#17462 = CARTESIAN_POINT ( 'NONE',  ( -13.18032351650865941, 35.03520933927575953, 2.969786570442512819 ) ) ;
#17463 = CARTESIAN_POINT ( 'NONE',  ( -13.49999999999999822, 21.08000000000001251, 4.386415899144235908 ) ) ;
#17464 = ORIENTED_EDGE ( 'NONE', *, *, #14402, .F. ) ;
#17465 = CARTESIAN_POINT ( 'NONE',  ( 0.000000000000000000, 80.93000000000000682, 0.000000000000000000 ) ) ;
#17466 = EDGE_CURVE ( 'NONE', #3534, #11272, #9658, .T. ) ;
#17467 = CARTESIAN_POINT ( 'NONE',  ( -5.632930873440789021, 31.38456733775239016, -12.26872874113417389 ) ) ;
#17468 = CARTESIAN_POINT ( 'NONE',  ( 5.789886819189885792, 72.96932708321882899, -12.19559009533250915 ) ) ;
#17469 = CARTESIAN_POINT ( 'NONE',  ( -7.272992578804310604, -10.62000000000000099, 10.01041549318726709 ) ) ;
#17470 = CARTESIAN_POINT ( 'NONE',  ( 3.015881606418733263, 59.78851020975074704, 13.15953674005853635 ) ) ;
#17471 = CARTESIAN_POINT ( 'NONE',  ( 4.171729424061791924, -6.969999999999997087, -12.83926296998457239 ) ) ;
#17472 = CARTESIAN_POINT ( 'NONE',  ( -10.89631187464833673, 53.23151712802560098, 7.970223035170421966 ) ) ;
#17473 = AXIS2_PLACEMENT_3D ( 'NONE', #8922, #602, #14281 ) ;
#17474 = CARTESIAN_POINT ( 'NONE',  ( 3.636496289402154414, 45.82999999999999829, 11.19198476289190936 ) ) ;
#17475 = CARTESIAN_POINT ( 'NONE',  ( -4.171729424061791036, 64.53000000000000114, 12.83926296998457239 ) ) ;
#17476 = CARTESIAN_POINT ( 'NONE',  ( 10.68961761359567397, 51.11669578649746626, 8.245125799009599632 ) ) ;
#17477 = CARTESIAN_POINT ( 'NONE',  ( -11.80778863418780666, 37.68739598817739278, -6.544568176179799579 ) ) ;
#17478 = CARTESIAN_POINT ( 'NONE',  ( 7.866617039688436286, 35.97691261133539342, 10.98018032865522109 ) ) ;
#17479 = CARTESIAN_POINT ( 'NONE',  ( -18.62500000000064659, -33.26562499999994316, 7.714727599197333419 ) ) ;
#17480 = CARTESIAN_POINT ( 'NONE',  ( -11.98344142294277148, 74.15943957762281968, 6.216689467641591804 ) ) ;
#17481 = CARTESIAN_POINT ( 'NONE',  ( -11.61371576356372692, 76.67242678379393794, -6.919319138424564919 ) ) ;
#17482 = CARTESIAN_POINT ( 'NONE',  ( -13.19914138750825749, 79.82943297964098406, -2.843127574936424651 ) ) ;
#17483 = CARTESIAN_POINT ( 'NONE',  ( -3.636496289402156190, 10.53000000000001180, 11.19198476289190758 ) ) ;
#17484 = CARTESIAN_POINT ( 'NONE',  ( -9.999999999999776179, 0.000000000000000000, -17.32050807568890605 ) ) ;
#17485 = CARTESIAN_POINT ( 'NONE',  ( 3.636496289402154414, 4.830000000000000959, 11.19198476289190758 ) ) ;
#17486 = CARTESIAN_POINT ( 'NONE',  ( -9.520470885617717371, 45.22999999999999687, 6.917026985038133624 ) ) ;
#17487 = CARTESIAN_POINT ( 'NONE',  ( 10.99999999999990941, 0.000000000000000000, 15.58845726811995824 ) ) ;
#17488 = NEXT_ASSEMBLY_USAGE_OCCURRENCE ( 'NAUO1', ' ', ' ', #8388, #8924, $ ) ;
#17489 = NEXT_ASSEMBLY_USAGE_OCCURRENCE ( 'NAUO2', ' ', ' ', #8388, #48, $ ) ;
#17490 = NEXT_ASSEMBLY_USAGE_OCCURRENCE ( 'NAUO3', ' ', ' ', #8388, #3168, $ ) ;
#17491 = NEXT_ASSEMBLY_USAGE_OCCURRENCE ( 'NAUO4', ' ', ' ', #8388, #3939, $ ) ;
#17492=COLOUR_RGB('Dark Blue',0.08,0.2,0.34);
#17493=FILL_AREA_STYLE_COLOUR('',#17492);
#17494=FILL_AREA_STYLE('',(#17493));
#17495=SURFACE_STYLE_FILL_AREA(#17494);
#17496=SURFACE_SIDE_STYLE('',(#17495));
#17497=SURFACE_STYLE_USAGE(.BOTH.,#17496);
#17498=PRESENTATION_STYLE_ASSIGNMENT((#17497));
#17499=COLOUR_RGB('Light Blue',0.38,0.62,0.78);
#17500=FILL_AREA_STYLE_COLOUR('',#17499);
#17501=FILL_AREA_STYLE('',(#17500));
#17502=SURFACE_STYLE_FILL_AREA(#17501);
#17503=SURFACE_SIDE_STYLE('',(#17502));
#17504=SURFACE_STYLE_USAGE(.BOTH.,#17503);
#17505=PRESENTATION_STYLE_ASSIGNMENT((#17504));
#17506=COLOUR_RGB('Sky Blue',0.24,0.69,0.87);
#17507=FILL_AREA_STYLE_COLOUR('',#17506);
#17508=FILL_AREA_STYLE('',(#17507));
#17509=SURFACE_STYLE_FILL_AREA(#17508);
#17510=SURFACE_SIDE_STYLE('',(#17509));
#17511=SURFACE_STYLE_USAGE(.BOTH.,#17510);
#17512=PRESENTATION_STYLE_ASSIGNMENT((#17511));
#17513=COLOUR_RGB('Grey',0.48,0.52,0.57);
#17514=FILL_AREA_STYLE_COLOUR('',#17513);
#17515=FILL_AREA_STYLE('',(#17514));
#17516=SURFACE_STYLE_FILL_AREA(#17515);
#17517=SURFACE_SIDE_STYLE('',(#17516));
#17518=SURFACE_STYLE_USAGE(.BOTH.,#17517);
#17519=PRESENTATION_STYLE_ASSIGNMENT((#17518));
#17520=COLOUR_RGB('Black',0.12,0.14,0.17);
#17521=FILL_AREA_STYLE_COLOUR('',#17520);
#17522=FILL_AREA_STYLE('',(#17521));
#17523=SURFACE_STYLE_FILL_AREA(#17522);
#17524=SURFACE_SIDE_STYLE('',(#17523));
#17525=SURFACE_STYLE_USAGE(.BOTH.,#17524);
#17526=PRESENTATION_STYLE_ASSIGNMENT((#17525));
#17527=COLOUR_RGB('Off White',0.89,0.88,0.83);
#17528=FILL_AREA_STYLE_COLOUR('',#17527);
#17529=FILL_AREA_STYLE('',(#17528));
#17530=SURFACE_STYLE_FILL_AREA(#17529);
#17531=SURFACE_SIDE_STYLE('',(#17530));
#17532=SURFACE_STYLE_USAGE(.BOTH.,#17531);
#17533=PRESENTATION_STYLE_ASSIGNMENT((#17532));
ENDSEC;
END-ISO-10303-21;
